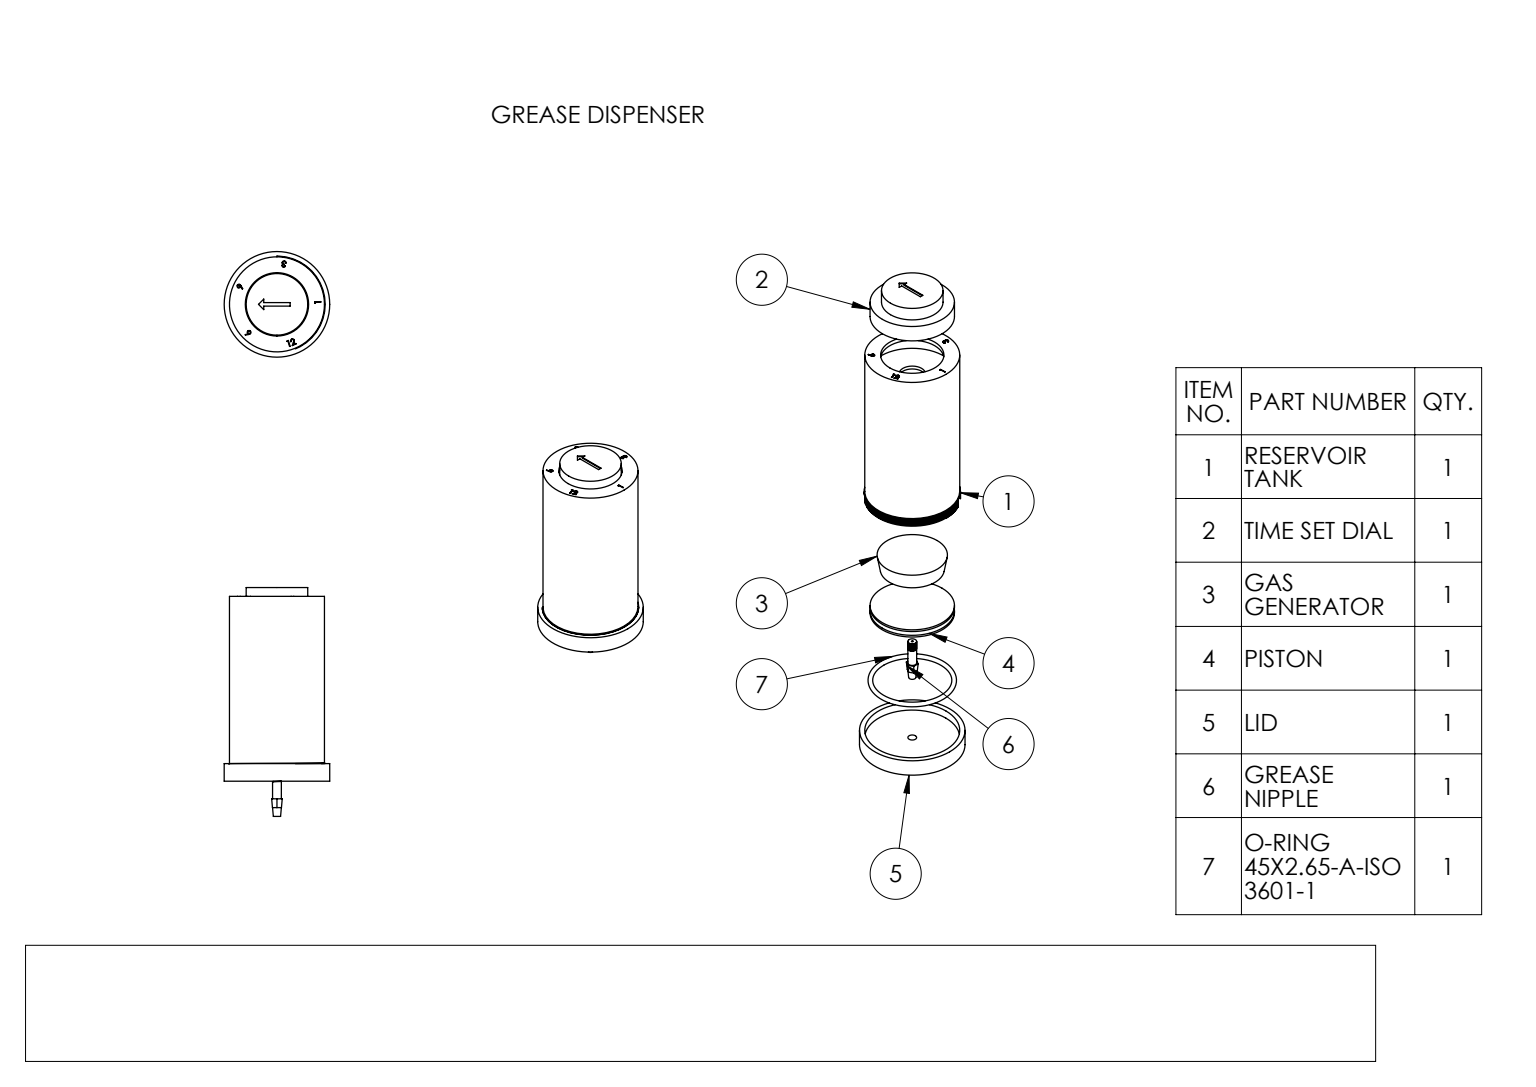
ISO-10303-21;
HEADER;
FILE_DESCRIPTION (('STEP AP214'),
    '1' );
FILE_NAME ('MAS-199',
    '2026-10-24T15:06:47',
    ( '' ),
    ( '' ),
    'SwSTEP 2.0',
    'SolidWorks 2026',
    '' );
FILE_SCHEMA (( 'AUTOMOTIVE_DESIGN' ));
ENDSEC;

DATA;
#1 = PRODUCT_DEFINITION_SHAPE ( 'NONE', 'NONE',  #7805 ) ;
#2 = CARTESIAN_POINT ( 'NONE',  ( 0.000000000000000000, 72.50000000000001421, 0.000000000000000000 ) ) ;
#3 = CARTESIAN_POINT ( 'NONE',  ( 4.786228327491940187E-16, -2.728124999385483473, 2.605501347177161087 ) ) ;
#4 = CARTESIAN_POINT ( 'NONE',  ( -22.08823018108446234, 99.50000000000000000, -9.406177930363766038 ) ) ;
#5 = ORIENTED_EDGE ( 'NONE', *, *, #2695, .F. ) ;
#6 = EDGE_LOOP ( 'NONE', ( #8139, #8496, #8983, #2392 ) ) ;
#7 = CARTESIAN_POINT ( 'NONE',  ( 2.256430356249999658, -2.578124999385483118, -1.302750673588581432 ) ) ;
#8 = CARTESIAN_POINT ( 'NONE',  ( 11.36312591709336850, 1.799999998907525267, 27.43301269999999903 ) ) ;
#9 = EDGE_CURVE ( 'NONE', #2280, #2682, #6327, .T. ) ;
#10 = FILL_AREA_STYLE_COLOUR ( '', #10270 ) ;
#11 = LINE ( 'NONE', #3942, #5600 ) ;
#12 = ADVANCED_FACE ( 'NONE', ( #17 ), #758, .T. ) ;
#13 = CARTESIAN_POINT ( 'NONE',  ( -27.00000000000001421, 4.450000000000000178, 11.18376618407356382 ) ) ;
#14 = DIRECTION ( 'NONE',  ( 0.3918949146621865109, 0.000000000000000000, 0.9200099868272720860 ) ) ;
#15 = CARTESIAN_POINT ( 'NONE',  ( -21.07742585509981126, 99.49999999999998579, -10.85999754779651383 ) ) ;
#16 = CARTESIAN_POINT ( 'NONE',  ( 1.128215178125001161, -4.153124999385482852, 1.954126010382870815 ) ) ;
#17 = FACE_OUTER_BOUND ( 'NONE', #3726, .T. ) ;
#18 = CARTESIAN_POINT ( 'NONE',  ( -11.36312591709335962, 2.899999998907525356, -27.43301270000000258 ) ) ;
#19 = CARTESIAN_POINT ( 'NONE',  ( 4.295198626299898237, 99.50000000000001421, -24.68029520312135361 ) ) ;
#20 = CARTESIAN_POINT ( 'NONE',  ( 1.249999999999999334, -1.050000000000000044, -2.165063509461096825 ) ) ;
#21 = CARTESIAN_POINT ( 'NONE',  ( 1.128215178124999607, -3.103124999385482585, -1.954126010382871259 ) ) ;
#22 = CYLINDRICAL_SURFACE ( 'NONE', #5038, 2.499999999999999556 ) ;
#23 = CARTESIAN_POINT ( 'NONE',  ( -22.51767453479306980, 100.0000000000000000, -9.764155749770198511 ) ) ;
#24 = FACE_OUTER_BOUND ( 'NONE', #4526, .T. ) ;
#25 = CARTESIAN_POINT ( 'NONE',  ( 1.250000000000001110, -2.043749998770965970, 2.165063509461096380 ) ) ;
#26 = VERTEX_POINT ( 'NONE', #3950 ) ;
#27 = CARTESIAN_POINT ( 'NONE',  ( 1.249999999999999334, -0.9937499987709658145, -2.165063509461096825 ) ) ;
#28 = CARTESIAN_POINT ( 'NONE',  ( -2.499999999999999112, -3.112499999999999822, 1.443375672974065882 ) ) ;
#29 = CARTESIAN_POINT ( 'NONE',  ( -14.97509118869195888, 99.99999999999998579, 15.26515554624281101 ) ) ;
#30 = CARTESIAN_POINT ( 'NONE',  ( 4.786228327491941173E-16, -3.178124999385482763, 2.605501347177161087 ) ) ;
#31 = ORIENTED_EDGE ( 'NONE', *, *, #3987, .F. ) ;
#32 = CIRCLE ( 'NONE', #8383, 30.00000000000000000 ) ;
#33 = AXIS2_PLACEMENT_3D ( 'NONE', #2920, #5329, #6943 ) ;
#34 = ORIENTED_EDGE ( 'NONE', *, *, #3622, .T. ) ;
#35 = CARTESIAN_POINT ( 'NONE',  ( -22.31230063665282515, 99.99999999999997158, -10.62159318200525249 ) ) ;
#36 = DIRECTION ( 'NONE',  ( 0.000000000000000000, 1.000000000000000000, 0.000000000000000000 ) ) ;
#37 = CARTESIAN_POINT ( 'NONE',  ( 1.034219503716432668E-14, -3.656249998770965792, -2.500000000000000000 ) ) ;
#38 = CARTESIAN_POINT ( 'NONE',  ( 27.00000000000000355, 2.999999997815050889, 0.000000000000000000 ) ) ;
#39 = CARTESIAN_POINT ( 'NONE',  ( 19.39806930854667399, 3.449999998907525622, 19.39806930854668465 ) ) ;
#40 = AXIS2_PLACEMENT_3D ( 'NONE', #3682, #8497, #6028 ) ;
#41 = EDGE_LOOP ( 'NONE', ( #10357, #6514, #2134, #4776 ) ) ;
#42 = EDGE_CURVE ( 'NONE', #3838, #8637, #9238, .T. ) ;
#43 = CARTESIAN_POINT ( 'NONE',  ( 3.739209042966563867, 99.50000000000000000, -21.42288334414699236 ) ) ;
#44 = ITEM_DEFINED_TRANSFORMATION ( 'NONE', 'NONE', #5307,  #5055 ) ;
#45 = CARTESIAN_POINT ( 'NONE',  ( 3.873456569393397331, 100.0000000000000284, -22.53291374702356364 ) ) ;
#46 = CARTESIAN_POINT ( 'NONE',  ( -2.256430356249999214, -3.365624999385482319, 1.302750673588581876 ) ) ;
#47 = CARTESIAN_POINT ( 'NONE',  ( -21.28703419482447146, 99.49999999999997158, -11.01737971290317297 ) ) ;
#48 = CARTESIAN_POINT ( 'NONE',  ( 11.36312591709336139, 5.299999998907526155, -27.43301270000000258 ) ) ;
#49 = UNCERTAINTY_MEASURE_WITH_UNIT (LENGTH_MEASURE( 1.000000000000000082E-05 ), #5358, 'distance_accuracy_value', 'NONE');
#50 = AXIS2_PLACEMENT_3D ( 'NONE', #9695, #1591, #1737 ) ;
#51 = CARTESIAN_POINT ( 'NONE',  ( -15.10382517959271098, 99.49999999999998579, 15.91526905993627317 ) ) ;
#52 = DIRECTION ( 'NONE',  ( 0.4750403377899758972, 0.000000000000000000, -0.8799640205556052974 ) ) ;
#53 = CARTESIAN_POINT ( 'NONE',  ( 0.000000000000000000, 85.00000000000000000, -20.00000000000000000 ) ) ;
#54 = CARTESIAN_POINT ( 'NONE',  ( 3.061616997868383141E-16, 0.000000000000000000, 2.500000000000000000 ) ) ;
#55 = CARTESIAN_POINT ( 'NONE',  ( -1.128215178124998497, -3.665624999385482585, 1.954126010382872147 ) ) ;
#56 = CARTESIAN_POINT ( 'NONE',  ( 9.910564025336874749, 100.0000000000000142, 20.75459158945058036 ) ) ;
#57 = ORIENTED_EDGE ( 'NONE', *, *, #3072, .T. ) ;
#58 = ADVANCED_FACE ( 'NONE', ( #3173 ), #2520, .T. ) ;
#59 = ORIENTED_EDGE ( 'NONE', *, *, #4217, .F. ) ;
#60 = CARTESIAN_POINT ( 'NONE',  ( -2.256430356250000102, -1.940624999385482941, 0.000000000000000000 ) ) ;
#61 = CARTESIAN_POINT ( 'NONE',  ( 27.43301270000000258, 1.999999998907524779, -11.36312591709336139 ) ) ;
#62 = FILL_AREA_STYLE ('',( #10 ) ) ;
#63 = CARTESIAN_POINT ( 'NONE',  ( 1.679787559701184688E-15, 5.249999998907525445, -27.43301270000000258 ) ) ;
#64 = AXIS2_PLACEMENT_3D ( 'NONE', #1231, #6667, #8456 ) ;
#65 = CARTESIAN_POINT ( 'NONE',  ( 11.18376618407356915, 4.950000000000000178, -27.00000000000000355 ) ) ;
#66 = FACE_OUTER_BOUND ( 'NONE', #7305, .T. ) ;
#67 = CARTESIAN_POINT ( 'NONE',  ( -16.33590634957226229, 99.50000000000000000, 16.80570853669505382 ) ) ;
#68 = CARTESIAN_POINT ( 'NONE',  ( -20.91264567078791714, 99.99999999999994316, -10.54226115003387676 ) ) ;
#69 = EDGE_CURVE ( 'NONE', #5685, #7937, #6333, .T. ) ;
#70 = ORIENTED_EDGE ( 'NONE', *, *, #9652, .T. ) ;
#71 = ORIENTED_EDGE ( 'NONE', *, *, #3469, .T. ) ;
#72 = CARTESIAN_POINT ( 'NONE',  ( 3.551917533706515417, 100.0000000000000142, -21.11785906961830150 ) ) ;
#73 = ORIENTED_EDGE ( 'NONE', *, *, #5083, .F. ) ;
#74 = ADVANCED_FACE ( 'NONE', ( #2725 ), #8325, .T. ) ;
#75 = CARTESIAN_POINT ( 'NONE',  ( 27.43301269999999548, 4.199999998907525622, 11.36312591709337916 ) ) ;
#76 = FACE_OUTER_BOUND ( 'NONE', #1497, .T. ) ;
#77 = CARTESIAN_POINT ( 'NONE',  ( 9.877377282685029372E-16, -1.237499999999999600, 2.500000000000000000 ) ) ;
#78 = CARTESIAN_POINT ( 'NONE',  ( 2.256430356250000546, -4.565624999385482496, 1.302750673588579877 ) ) ;
#79 = CARTESIAN_POINT ( 'NONE',  ( -4.357666448243394824E-15, -2.531249998770965348, 2.500000000000000000 ) ) ;
#80 = EDGE_CURVE ( 'NONE', #2765, #6040, #6971, .T. ) ;
#81 = CARTESIAN_POINT ( 'NONE',  ( -22.63784607493503387, 99.50000000000001421, -10.71517552924587058 ) ) ;
#82 = AXIS2_PLACEMENT_3D ( 'NONE', #9543, #4773, #8119 ) ;
#83 = CARTESIAN_POINT ( 'NONE',  ( -1.250000000000000222, -4.518749998770965171, -2.165063509461096825 ) ) ;
#84 = VERTEX_POINT ( 'NONE', #3619 ) ;
#85 = EDGE_CURVE ( 'NONE', #5894, #5272, #1155, .T. ) ;
#86 = CARTESIAN_POINT ( 'NONE',  ( 1.653273178848927064E-15, 2.399999997815050357, -27.00000000000000355 ) ) ;
#87 = CARTESIAN_POINT ( 'NONE',  ( -20.71654887124055122, 99.50000000000001421, -9.874326132881018125 ) ) ;
#88 = LINE ( 'NONE', #2497, #4362 ) ;
#89 = CARTESIAN_POINT ( 'NONE',  ( 2.256430356249999658, -3.928124999385482319, -1.302750673588581432 ) ) ;
#90 = B_SPLINE_SURFACE_WITH_KNOTS ( 'NONE', 3, 1, ( 
 ( #3080, #5199 ),
 ( #8397, #1229 ),
 ( #4422, #5539 ),
 ( #1701, #10302 ),
 ( #3282, #3232 ),
 ( #4117, #7200 ),
 ( #3911, #924 ),
 ( #4848, #7097 ),
 ( #4064, #3134 ),
 ( #2291, #2443 ),
 ( #6321, #139 ) ),
 .UNSPECIFIED., .F., .F., .F.,
 ( 4, 1, 1, 1, 1, 1, 1, 1, 4 ),
 ( 2, 2 ),
 ( 0.000000000000000000, 0.09809051273808343241, 0.1997563395654988194, 0.3058527769869914259, 0.4162847437678430240, 0.5377099880548563693, 0.6743560419832976827, 0.8289895874771281425, 1.000000000000000000 ),
 ( 0.000000000000000000, 1.000000000000000000 ),
 .UNSPECIFIED. ) ;
#91 = CARTESIAN_POINT ( 'NONE',  ( 3.058419780146050648, 99.50000000000000000, -23.12871267107006545 ) ) ;
#92 = ORIENTED_EDGE ( 'NONE', *, *, #2350, .T. ) ;
#93 = AXIS2_PLACEMENT_3D ( 'NONE', #4532, #670, #7729 ) ;
#94 = CARTESIAN_POINT ( 'NONE',  ( -15.22320097062094568, 99.50000000000001421, 16.32303119091969634 ) ) ;
#95 = CARTESIAN_POINT ( 'NONE',  ( -2.499999999999999112, -3.506249998770964993, 1.443375672974065882 ) ) ;
#96 = CARTESIAN_POINT ( 'NONE',  ( 0.000000000000000000, 100.0000000000000000, 0.000000000000000000 ) ) ;
#97 = CARTESIAN_POINT ( 'NONE',  ( 9.245739950628269810, 100.0000000000000284, 20.03726560014620617 ) ) ;
#98 = ORIENTED_EDGE ( 'NONE', *, *, #7857, .T. ) ;
#99 = CARTESIAN_POINT ( 'NONE',  ( 0.000000000000000000, 0.000000000000000000, 0.000000000000000000 ) ) ;
#100 = VECTOR ( 'NONE', #6339, 1000.000000000000000 ) ;
#101 = CARTESIAN_POINT ( 'NONE',  ( -20.89169796687544789, 100.0000000000000142, -10.40078880447404330 ) ) ;
#102 = CARTESIAN_POINT ( 'NONE',  ( -2.256430356250000102, -0.1781249993854829572, -1.302750673588580321 ) ) ;
#103 = EDGE_CURVE ( 'NONE', #3372, #2494, #7434, .T. ) ;
#104 = FACE_OUTER_BOUND ( 'NONE', #9219, .T. ) ;
#105 = CARTESIAN_POINT ( 'NONE',  ( 27.43301269999999548, 5.099999998907525978, 11.36312591709337738 ) ) ;
#106 = CARTESIAN_POINT ( 'NONE',  ( -15.19031985176477662, 99.49999999999998579, 15.56880617076518547 ) ) ;
#107 = DIRECTION ( 'NONE',  ( 0.000000000000000000, 0.000000000000000000, 1.000000000000000000 ) ) ;
#108 = CARTESIAN_POINT ( 'NONE',  ( -15.37123125604856710, 99.50000000000001421, 16.48683530611566539 ) ) ;
#109 = DIRECTION ( 'NONE',  ( 4.336808689942017736E-16, 0.000000000000000000, -1.000000000000000000 ) ) ;
#110 = CARTESIAN_POINT ( 'NONE',  ( -1.128215178124998497, -4.115624999385482319, 1.954126010382872147 ) ) ;
#111 = CARTESIAN_POINT ( 'NONE',  ( 3.970307086022987431, 99.50000000000001421, -24.36314111580913178 ) ) ;
#112 = EDGE_LOOP ( 'NONE', ( #9331, #6596, #10060, #487 ) ) ;
#113 = ORIENTED_EDGE ( 'NONE', *, *, #6148, .T. ) ;
#114 = CARTESIAN_POINT ( 'NONE',  ( -1.128215178124998497, -3.665624999385482585, 1.954126010382872147 ) ) ;
#115 = CARTESIAN_POINT ( 'NONE',  ( 27.43301270000000258, 1.149999998907525356, 0.000000000000000000 ) ) ;
#116 = CARTESIAN_POINT ( 'NONE',  ( 0.000000000000000000, 0.000000000000000000, 0.000000000000000000 ) ) ;
#117 = FACE_OUTER_BOUND ( 'NONE', #7334, .T. ) ;
#118 = CARTESIAN_POINT ( 'NONE',  ( -27.43301270000000258, 0.6499999989075253559, -3.359575119402369376E-15 ) ) ;
#119 = DIRECTION ( 'NONE',  ( -0.000000000000000000, -1.000000000000000000, -0.000000000000000000 ) ) ;
#120 = ORIENTED_EDGE ( 'NONE', *, *, #3091, .T. ) ;
#121 = EDGE_CURVE ( 'NONE', #3756, #7561, #4966, .T. ) ;
#122 = VECTOR ( 'NONE', #1890, 999.9999999999998863 ) ;
#123 = CARTESIAN_POINT ( 'NONE',  ( 0.000000000000000000, 99.50000000000000000, 0.000000000000000000 ) ) ;
#124 = FACE_OUTER_BOUND ( 'NONE', #10204, .T. ) ;
#125 = ORIENTED_EDGE ( 'NONE', *, *, #7390, .T. ) ;
#126 = ORIENTED_EDGE ( 'NONE', *, *, #1417, .F. ) ;
#127 = CARTESIAN_POINT ( 'NONE',  ( 1.250000000000001110, -5.193749998770964993, 2.165063509461096380 ) ) ;
#128 = CARTESIAN_POINT ( 'NONE',  ( 19.39806930854667399, 4.949999998907525622, 19.39806930854668465 ) ) ;
#129 = CARTESIAN_POINT ( 'NONE',  ( 3.538198506519217190, 99.99999999999998579, -24.58220198924426114 ) ) ;
#130 = CARTESIAN_POINT ( 'NONE',  ( -2.256430356250000102, -4.303124999385482319, 0.000000000000000000 ) ) ;
#131 = CARTESIAN_POINT ( 'NONE',  ( -16.49419651247312046, 99.99999999999998579, 15.57134447358898477 ) ) ;
#132 = CARTESIAN_POINT ( 'NONE',  ( -22.69253165798458127, 100.0000000000000142, -10.28928739654909563 ) ) ;
#133 = CARTESIAN_POINT ( 'NONE',  ( 4.331079892889020400, 100.0000000000000000, -24.67336562508343079 ) ) ;
#134 = AXIS2_PLACEMENT_3D ( 'NONE', #8588, #6169, #2769 ) ;
#135 = CARTESIAN_POINT ( 'NONE',  ( -1.249999999999998224, -4.368749998770964815, 2.165063509461097713 ) ) ;
#136 = ORIENTED_EDGE ( 'NONE', *, *, #3638, .F. ) ;
#137 = ORIENTED_EDGE ( 'NONE', *, *, #6348, .F. ) ;
#138 = FACE_OUTER_BOUND ( 'NONE', #6423, .T. ) ;
#139 = CARTESIAN_POINT ( 'NONE',  ( -16.07368679829020763, 100.0000000000000000, 17.11560437002838952 ) ) ;
#140 = CARTESIAN_POINT ( 'NONE',  ( -14.74935495356232984, 100.0000000000000142, 15.91322402822111926 ) ) ;
#141 = CARTESIAN_POINT ( 'NONE',  ( -1.128215178125000273, -3.815624999385482941, -1.954126010382871259 ) ) ;
#142 = ADVANCED_FACE ( 'NONE', ( #1039 ), #6680, .T. ) ;
#143 = EDGE_CURVE ( 'NONE', #8324, #1908, #2115, .T. ) ;
#144 = AXIS2_PLACEMENT_3D ( 'NONE', #2203, #6849, #5404 ) ;
#145 = LINE ( 'NONE', #6521, #2502 ) ;
#146 = DIRECTION ( 'NONE',  ( -1.000000000000000000, -0.000000000000000000, -0.000000000000000000 ) ) ;
#147 = CARTESIAN_POINT ( 'NONE',  ( 1.250000000000001110, -3.843749998770965348, 2.165063509461096380 ) ) ;
#148 = CARTESIAN_POINT ( 'NONE',  ( -19.09188309203678813, 4.500000000000000888, 19.09188309203678457 ) ) ;
#149 = EDGE_LOOP ( 'NONE', ( #7106, #3257, #2787, #8826 ) ) ;
#150 = CARTESIAN_POINT ( 'NONE',  ( 3.411785164761435674, 99.50000000000000000, -22.76693382491622231 ) ) ;
#151 = CARTESIAN_POINT ( 'NONE',  ( 3.750007936853901658, 99.99999999999998579, -22.95001988029826734 ) ) ;
#152 = CARTESIAN_POINT ( 'NONE',  ( 7.856939908706818798, 99.50000000000001421, 20.19612520319305560 ) ) ;
#153 = DIRECTION ( 'NONE',  ( -0.000000000000000000, -0.000000000000000000, -1.000000000000000000 ) ) ;
#154 = CARTESIAN_POINT ( 'NONE',  ( 27.43301270000000258, 4.349999998907525089, 0.000000000000000000 ) ) ;
#155 = CARTESIAN_POINT ( 'NONE',  ( 26.99999999999999645, 3.150000000000000799, 11.18376618407358691 ) ) ;
#156 = CARTESIAN_POINT ( 'NONE',  ( -21.24882413972086681, 100.0000000000000284, -9.742484589929601313 ) ) ;
#157 = CARTESIAN_POINT ( 'NONE',  ( 3.717146347979291665, 99.50000000000000000, -21.42716062222556417 ) ) ;
#158 = CARTESIAN_POINT ( 'NONE',  ( 3.681717055787076642, 99.50000000000000000, -21.09125273517263111 ) ) ;
#159 = CARTESIAN_POINT ( 'NONE',  ( 1.034219503716432668E-14, -4.612500000000000711, -2.500000000000000000 ) ) ;
#160 = ORIENTED_EDGE ( 'NONE', *, *, #2379, .T. ) ;
#161 = CARTESIAN_POINT ( 'NONE',  ( -2.256430356249999214, -4.153124999385482852, 1.302750673588581876 ) ) ;
#162 = CARTESIAN_POINT ( 'NONE',  ( -16.01161620991261358, 99.50000000000000000, 17.10240122391520146 ) ) ;
#163 = B_SPLINE_CURVE_WITH_KNOTS ( 'NONE', 3,
 ( #932, #5497, #832, #3193, #8885, #3093, #3922, #8786, #6277, #3240, #8737, #729, #9473, #2452, #4752 ),
 .UNSPECIFIED., .F., .F.,
 ( 4, 1, 1, 1, 1, 1, 1, 1, 1, 1, 1, 1, 4 ),
 ( 0.000000000000000000, 0.08490232564366416435, 0.1680779112633816463, 0.2506304657828534177, 0.3338427399641299420, 0.4169763759729993580, 0.4990117930239920674, 0.5811067191809071719, 0.6656374296971073745, 0.7500328835558887075, 0.8331455368193440014, 0.9159638734519762737, 1.000000000000000000 ),
 .UNSPECIFIED. ) ;
#164 = CARTESIAN_POINT ( 'NONE',  ( 11.18376618407357626, 3.049999999999999822, 27.00000000000000000 ) ) ;
#165 = CARTESIAN_POINT ( 'NONE',  ( 3.373335371007685435, 99.50000000000000000, -22.75111425220066863 ) ) ;
#166 = CARTESIAN_POINT ( 'NONE',  ( 6.307557144418638510E-17, -20.00000000000000000, -2.958985580760425727 ) ) ;
#167 = CARTESIAN_POINT ( 'NONE',  ( 1.250000000000001110, -3.449999999999999289, 2.165063509461096380 ) ) ;
#168 = CARTESIAN_POINT ( 'NONE',  ( -21.07742585509981126, 99.99999999999995737, -10.85999754779651383 ) ) ;
#169 = ORIENTED_EDGE ( 'NONE', *, *, #6403, .F. ) ;
#170 = CARTESIAN_POINT ( 'NONE',  ( 1.249999999999999334, -1.443749998770965881, -2.165063509461096825 ) ) ;
#171 = CARTESIAN_POINT ( 'NONE',  ( 2.500000000000000000, -4.218749998770966236, -3.061616997868383141E-16 ) ) ;
#172 = EDGE_CURVE ( 'NONE', #957, #2983, #5656, .T. ) ;
#173 = CARTESIAN_POINT ( 'NONE',  ( -1.128215178125000273, -4.828124999385481786, -1.954126010382871259 ) ) ;
#174 = CARTESIAN_POINT ( 'NONE',  ( 9.404665101723468368, 99.50000000000000000, 20.17141824467128686 ) ) ;
#175 = CARTESIAN_POINT ( 'NONE',  ( -16.87593989452418697, 99.49999999999998579, 15.58794934546231126 ) ) ;
#176 = CARTESIAN_POINT ( 'NONE',  ( 8.064245308217579122, 99.99999999999998579, 20.64099956338070641 ) ) ;
#177 = SHAPE_REPRESENTATION ( 'piston', ( #5055 ), #738 ) ;
#178 = CARTESIAN_POINT ( 'NONE',  ( -1.250000000000000222, -3.618749998770965259, -2.165063509461096825 ) ) ;
#179 = ORIENTED_EDGE ( 'NONE', *, *, #6506, .T. ) ;
#180 = ORIENTED_EDGE ( 'NONE', *, *, #3035, .T. ) ;
#181 = EDGE_CURVE ( 'NONE', #471, #3838, #8521, .T. ) ;
#182 = CARTESIAN_POINT ( 'NONE',  ( -22.29247428061501779, 99.99999999999997158, -10.66603791136541624 ) ) ;
#183 = CARTESIAN_POINT ( 'NONE',  ( 3.611424427577684781, 99.99999999999998579, -21.45475674085064099 ) ) ;
#184 = EDGE_CURVE ( 'NONE', #533, #5989, #307, .T. ) ;
#185 = CARTESIAN_POINT ( 'NONE',  ( -15.07178375341841381, 100.0000000000000000, 16.66969090848992607 ) ) ;
#186 = CARTESIAN_POINT ( 'NONE',  ( 1.128215178125001161, -4.490624999385482319, 1.954126010382870815 ) ) ;
#187 = ORIENTED_EDGE ( 'NONE', *, *, #7681, .T. ) ;
#188 = DIRECTION ( 'NONE',  ( 0.000000000000000000, -1.000000000000000000, 0.000000000000000000 ) ) ;
#189 = PRODUCT_RELATED_PRODUCT_CATEGORY ( 'part', '', ( #8779 ) ) ;
#190 = DIRECTION ( 'NONE',  ( -0.05422338932609765960, 0.000000000000000000, -0.9985288298541962204 ) ) ;
#191 = EDGE_CURVE ( 'NONE', #3656, #1900, #9595, .T. ) ;
#192 = PLANE ( 'NONE',  #10324 ) ;
#193 = ORIENTED_EDGE ( 'NONE', *, *, #8350, .T. ) ;
#194 = ADVANCED_FACE ( 'NONE', ( #1864 ), #9727, .F. ) ;
#195 = CARTESIAN_POINT ( 'NONE',  ( 3.302864939465488536, 99.50000000000001421, -22.83905924565489443 ) ) ;
#196 = CARTESIAN_POINT ( 'NONE',  ( 3.891852272358404807, 99.99999999999998579, -22.89765557720719968 ) ) ;
#197 = CARTESIAN_POINT ( 'NONE',  ( 6.123233995736709336E-17, -25.00000000000000000, 0.4999999999999953371 ) ) ;
#198 = EDGE_LOOP ( 'NONE', ( #2371, #2144, #704, #4706 ) ) ;
#199 = CARTESIAN_POINT ( 'NONE',  ( 3.207057600658871355, 100.0000000000000284, -22.07913334414698880 ) ) ;
#200 = CARTESIAN_POINT ( 'NONE',  ( 27.00000000000000355, 2.999999997815050889, 0.000000000000000000 ) ) ;
#201 = CARTESIAN_POINT ( 'NONE',  ( -20.71654887124055122, 100.0000000000000142, -9.874326132881018125 ) ) ;
#202 = CARTESIAN_POINT ( 'NONE',  ( -21.66466628782423243, 100.0000000000000142, -9.640935998098070669 ) ) ;
#203 = LINE ( 'NONE', #3388, #8398 ) ;
#204 = VECTOR ( 'NONE', #9185, 1000.000000000000000 ) ;
#205 = LINE ( 'NONE', #1725, #6091 ) ;
#206 = CARTESIAN_POINT ( 'NONE',  ( -0.6698729810778081273, -2.157596189432334111, 2.499999999999999112 ) ) ;
#207 = ORIENTED_EDGE ( 'NONE', *, *, #9006, .F. ) ;
#208 = CARTESIAN_POINT ( 'NONE',  ( 2.256430356250000546, -4.003124999385482496, 1.302750673588579877 ) ) ;
#209 = FACE_OUTER_BOUND ( 'NONE', #3870, .T. ) ;
#210 = CARTESIAN_POINT ( 'NONE',  ( 9.806436918512124734, 99.99999999999998579, 20.18080982695387604 ) ) ;
#211 = VECTOR ( 'NONE', #9822, 1000.000000000000000 ) ;
#212 = CARTESIAN_POINT ( 'NONE',  ( -27.43301270000000258, 2.199999998907525622, -11.36312591709336317 ) ) ;
#213 = CARTESIAN_POINT ( 'NONE',  ( 2.500000000000000000, -0.6187499987709659255, -3.061616997868383141E-16 ) ) ;
#214 = DIRECTION ( 'NONE',  ( -0.000000000000000000, 1.000000000000000000, -0.000000000000000000 ) ) ;
#215 = CARTESIAN_POINT ( 'NONE',  ( 8.429066232339796017, 100.0000000000000000, 19.67794530653910101 ) ) ;
#216 = CARTESIAN_POINT ( 'NONE',  ( 1.653273178848927064E-15, 2.399999997815050357, -27.00000000000000355 ) ) ;
#217 = ORIENTED_EDGE ( 'NONE', *, *, #7917, .F. ) ;
#218 = CARTESIAN_POINT ( 'NONE',  ( -20.89052720883767122, 99.50000000000000000, -9.602653601535816819 ) ) ;
#219 = CARTESIAN_POINT ( 'NONE',  ( 11.36312591709336139, 5.199999998907525622, -27.43301270000000258 ) ) ;
#220 = CARTESIAN_POINT ( 'NONE',  ( -16.18965924272485779, 99.49999999999998579, 15.26525457555968224 ) ) ;
#221 = FACE_OUTER_BOUND ( 'NONE', #8631, .T. ) ;
#222 = CARTESIAN_POINT ( 'NONE',  ( 2.500000000000000444, -2.456249998770965615, 1.443375672974063439 ) ) ;
#223 = CARTESIAN_POINT ( 'NONE',  ( 26.99999999999999645, 1.550000000000000266, 11.18376618407358691 ) ) ;
#224 = VERTEX_POINT ( 'NONE', #1816 ) ;
#225 = CARTESIAN_POINT ( 'NONE',  ( 5.240996349771887886, 100.0000000000000142, -23.60769396873743631 ) ) ;
#226 = ORIENTED_EDGE ( 'NONE', *, *, #3625, .T. ) ;
#227 = EDGE_CURVE ( 'NONE', #6767, #4694, #1090, .T. ) ;
#228 = CARTESIAN_POINT ( 'NONE',  ( 1.249999999999999334, -5.043749998770965526, -2.165063509461096825 ) ) ;
#229 = VERTEX_POINT ( 'NONE', #4281 ) ;
#230 = ORIENTED_EDGE ( 'NONE', *, *, #6289, .F. ) ;
#231 = LINE ( 'NONE', #3414, #2289 ) ;
#232 = LINE ( 'NONE', #8144, #5785 ) ;
#233 = CARTESIAN_POINT ( 'NONE',  ( -22.11394672483139701, 99.50000000000000000, -10.91855052283267646 ) ) ;
#234 =( BOUNDED_CURVE ( )  B_SPLINE_CURVE ( 1, ( #10186, #707 ),
 .UNSPECIFIED., .F., .F. ) 
 B_SPLINE_CURVE_WITH_KNOTS ( ( 2, 2 ),
 ( 0.000000000000000000, 1.000000000000000000 ),
 .UNSPECIFIED. ) 
 CURVE ( )  GEOMETRIC_REPRESENTATION_ITEM ( )  RATIONAL_B_SPLINE_CURVE ( ( 0.9401538480137057174, 0.9401538480137057174 ) ) 
 REPRESENTATION_ITEM ( '' )  );
#235 = CARTESIAN_POINT ( 'NONE',  ( -15.26676860252058887, 99.99999999999998579, 16.38168943497750973 ) ) ;
#236 = VECTOR ( 'NONE', #2101, 1000.000000000000000 ) ;
#237 = EDGE_CURVE ( 'NONE', #1790, #7639, #6949, .T. ) ;
#238 = DIRECTION ( 'NONE',  ( 0.000000000000000000, 0.000000000000000000, -1.000000000000000000 ) ) ;
#239 = DIRECTION ( 'NONE',  ( 0.000000000000000000, -1.000000000000000000, 0.000000000000000000 ) ) ;
#240 = CARTESIAN_POINT ( 'NONE',  ( 0.000000000000000000, 97.50000000000000000, 18.00000000000000000 ) ) ;
#241 = ORIENTED_EDGE ( 'NONE', *, *, #4209, .F. ) ;
#242 = CARTESIAN_POINT ( 'NONE',  ( 3.058419780146050648, 99.50000000000000000, -23.12871267107006545 ) ) ;
#243 = LINE ( 'NONE', #5946, #5211 ) ;
#244 = CARTESIAN_POINT ( 'NONE',  ( 3.701176614148623756, 99.50000000000000000, -24.64875008328975170 ) ) ;
#245 = CARTESIAN_POINT ( 'NONE',  ( 7.734522023158566739, 99.50000000000002842, 20.86022014488863618 ) ) ;
#246 = ORIENTED_EDGE ( 'NONE', *, *, #1140, .T. ) ;
#247 = CARTESIAN_POINT ( 'NONE',  ( 0.000000000000000000, 73.81339255365637086, 0.000000000000000000 ) ) ;
#248 = CARTESIAN_POINT ( 'NONE',  ( 1.653273178848927064E-15, 4.799999997815051600, -27.00000000000000355 ) ) ;
#249 = CARTESIAN_POINT ( 'NONE',  ( -21.00001322343447541, 99.50000000000001421, -9.990026185521596602 ) ) ;
#250 = CARTESIAN_POINT ( 'NONE',  ( 3.635130212803377781, 100.0000000000000000, -23.00575896550913768 ) ) ;
#251 = CARTESIAN_POINT ( 'NONE',  ( -21.72555844818415594, 99.50000000000001421, -11.09629251537910655 ) ) ;
#252 = CARTESIAN_POINT ( 'NONE',  ( 4.906732565843439531, 100.0000000000000142, -23.57187248890526376 ) ) ;
#253 = CARTESIAN_POINT ( 'NONE',  ( -1.250000000000000222, -2.324999999999999734, -2.165063509461096825 ) ) ;
#254 = VECTOR ( 'NONE', #2667, 1000.000000000000000 ) ;
#255 = B_SPLINE_CURVE_WITH_KNOTS ( 'NONE', 3,
 ( #43, #4128, #5748, #6482, #981, #3244, #8984, #8105, #7258, #4950, #7354, #5651, #9812, #9671, #7311 ),
 .UNSPECIFIED., .F., .F.,
 ( 4, 1, 1, 1, 1, 1, 1, 1, 1, 1, 1, 1, 4 ),
 ( 0.000000000000000000, 0.1166921615859537187, 0.2277195327244859735, 0.3361971884410420164, 0.4453256767247914527, 0.5018483577356800396, 0.5617326728321133666, 0.6243107931132723110, 0.6909729641497043273, 0.7615676753376537933, 0.8363829297815326136, 0.9156607463298391814, 0.9999999999999998890 ),
 .UNSPECIFIED. ) ;
#256 = CARTESIAN_POINT ( 'NONE',  ( -2.256430356250000546, -5.114265350234221685, -0.8212662131217605133 ) ) ;
#257 = SURFACE_STYLE_USAGE ( .BOTH. , #8210 ) ;
#258 = CARTESIAN_POINT ( 'NONE',  ( -15.03963071504896121, 100.0000000000000000, 16.63526396357264758 ) ) ;
#259 = CIRCLE ( 'NONE', #7786, 2.500000000000000000 ) ;
#260 = CARTESIAN_POINT ( 'NONE',  ( 0.000000000000000000, 5.000000000000000000, -30.00000000000000000 ) ) ;
#261 = CARTESIAN_POINT ( 'NONE',  ( 27.43301270000000258, 1.849999998907525534, 0.000000000000000000 ) ) ;
#262 = LINE ( 'NONE', #2027, #6876 ) ;
#263 = ADVANCED_FACE ( 'NONE', ( #4540 ), #1407, .T. ) ;
#264 = CARTESIAN_POINT ( 'NONE',  ( -20.64578974631102426, 99.99999999999995737, -10.10077944494247504 ) ) ;
#265 = DIRECTION ( 'NONE',  ( -0.000000000000000000, 1.000000000000000000, -0.000000000000000000 ) ) ;
#266 = CARTESIAN_POINT ( 'NONE',  ( 8.322475189980043098, 100.0000000000000142, 19.72675386960232657 ) ) ;
#267 = ORIENTED_EDGE ( 'NONE', *, *, #2370, .F. ) ;
#268 = CARTESIAN_POINT ( 'NONE',  ( -21.30033281797529909, 99.50000000000002842, -9.345151174687854834 ) ) ;
#269 = CARTESIAN_POINT ( 'NONE',  ( 4.135809822336132591, 99.99999999999998579, -24.70305975188825443 ) ) ;
#270 = DIRECTION ( 'NONE',  ( 0.000000000000000000, -1.000000000000000000, 0.000000000000000000 ) ) ;
#271 = CARTESIAN_POINT ( 'NONE',  ( 3.775125937424839151, 100.0000000000000000, -21.41825520325024712 ) ) ;
#272 = CARTESIAN_POINT ( 'NONE',  ( 8.829292973371666520, 99.49999999999998579, 19.92220432019063736 ) ) ;
#273 = CARTESIAN_POINT ( 'NONE',  ( 0.000000000000000000, 0.000000000000000000, -2.500000000000000000 ) ) ;
#274 = CIRCLE ( 'NONE', #2111, 2.499999999999999556 ) ;
#275 = CARTESIAN_POINT ( 'NONE',  ( 0.000000000000000000, 75.00000000000001421, 0.000000000000000000 ) ) ;
#276 = CARTESIAN_POINT ( 'NONE',  ( 4.786228327491941173E-16, -0.5906249993854828517, 2.605501347177161087 ) ) ;
#277 = ORIENTED_EDGE ( 'NONE', *, *, #5688, .F. ) ;
#278 = ORIENTED_EDGE ( 'NONE', *, *, #3961, .T. ) ;
#279 = VECTOR ( 'NONE', #5092, 1000.000000000000000 ) ;
#280 = CYLINDRICAL_SURFACE ( 'NONE', #8136, 0.4999999999999953371 ) ;
#281 = CARTESIAN_POINT ( 'NONE',  ( 6.246869686064662197, 99.50000000000000000, 20.92172973853146090 ) ) ;
#282 = CARTESIAN_POINT ( 'NONE',  ( 1.653273178848927064E-15, 4.799999997815051600, -27.00000000000000355 ) ) ;
#283 = DIRECTION ( 'NONE',  ( 8.881784197001252323E-16, 0.000000000000000000, 1.000000000000000000 ) ) ;
#284 = COLOUR_RGB ( '',1.000000000000000000, 0.9490196078431372140, 0.9098039215686274384 ) ;
#285 = CARTESIAN_POINT ( 'NONE',  ( 8.081885929396888102, 99.50000000000001421, 20.89785832093561169 ) ) ;
#286 = CARTESIAN_POINT ( 'NONE',  ( 2.852289972453743161, 99.50000000000000000, -22.14293542748032451 ) ) ;
#287 = CARTESIAN_POINT ( 'NONE',  ( 3.061616997868383141E-16, 0.000000000000000000, 2.500000000000000000 ) ) ;
#288 = CARTESIAN_POINT ( 'NONE',  ( 3.735769352376668184, 99.49999999999998579, -24.30643046864489420 ) ) ;
#289 =( BOUNDED_CURVE ( )  B_SPLINE_CURVE ( 2, ( #364, #2666, #6794, #9834, #213, #3555, #2617, #5222, #2774 ),
 .UNSPECIFIED., .F., .F. ) 
 B_SPLINE_CURVE_WITH_KNOTS ( ( 3, 2, 2, 2, 3 ),
 ( 0.02083333333333333218, 0.02777777777777777624, 0.04166666666666666435, 0.05555555555555555247, 0.06250000000000000000 ),
 .UNSPECIFIED. ) 
 CURVE ( )  GEOMETRIC_REPRESENTATION_ITEM ( )  RATIONAL_B_SPLINE_CURVE ( ( 0.9330127018922194093, 0.9330127018922194093, 1.000000000000000000, 0.8660254037844387076, 1.000000000000000000, 0.8660254037844387076, 1.000000000000000000, 0.9330127018922194093, 0.9330127018922194093 ) ) 
 REPRESENTATION_ITEM ( '' )  );
#290 = ORIENTED_EDGE ( 'NONE', *, *, #2409, .F. ) ;
#291 = DIRECTION ( 'NONE',  ( -0.000000000000000000, 1.000000000000000000, -0.000000000000000000 ) ) ;
#292 = CARTESIAN_POINT ( 'NONE',  ( -27.43301270000000258, 3.949999998907525178, -3.359575119402369376E-15 ) ) ;
#293 = CARTESIAN_POINT ( 'NONE',  ( -0.6698729810778054627, -2.101346188203299548, 2.500000000000000000 ) ) ;
#294 = EDGE_CURVE ( 'NONE', #8788, #5320, #3852, .T. ) ;
#295 = CIRCLE ( 'NONE', #9511, 17.50000000000000355 ) ;
#296 = DIRECTION ( 'NONE',  ( -0.000000000000000000, -1.000000000000000000, -0.000000000000000000 ) ) ;
#297 = CARTESIAN_POINT ( 'NONE',  ( 7.771508748547515388, 99.50000000000001421, 20.40818475981234315 ) ) ;
#298 = ORIENTED_EDGE ( 'NONE', *, *, #7410, .F. ) ;
#299 = CARTESIAN_POINT ( 'NONE',  ( 9.902568905804752575, 99.49999999999998579, 20.48863403721516363 ) ) ;
#300 = CARTESIAN_POINT ( 'NONE',  ( -11.18376618407356560, 3.249999997815050001, -27.00000000000000355 ) ) ;
#301 = CARTESIAN_POINT ( 'NONE',  ( -21.16695614262292580, 99.50000000000000000, -11.33496398805607441 ) ) ;
#302 = DIRECTION ( 'NONE',  ( -0.000000000000000000, -0.000000000000000000, -1.000000000000000000 ) ) ;
#303 = PRESENTATION_STYLE_ASSIGNMENT (( #1913 ) ) ;
#304 = CARTESIAN_POINT ( 'NONE',  ( -21.44539290152690114, 100.0000000000000000, -11.08070480119962298 ) ) ;
#305 = AXIS2_PLACEMENT_3D ( 'NONE', #9568, #7104, #7052 ) ;
#306 = PLANE ( 'NONE',  #2619 ) ;
#307 = LINE ( 'NONE', #5759, #1112 ) ;
#308 = ORIENTED_EDGE ( 'NONE', *, *, #1549, .F. ) ;
#309 = CARTESIAN_POINT ( 'NONE',  ( 5.302876193624534821E-16, -0.3375000000000000222, 2.886751345948128655 ) ) ;
#310 = EDGE_CURVE ( 'NONE', #1877, #7747, #8787, .T. ) ;
#311 = CARTESIAN_POINT ( 'NONE',  ( -2.499999999999999112, -2.662500000000000089, 1.443375672974065882 ) ) ;
#312 = CARTESIAN_POINT ( 'NONE',  ( -2.256430356250000102, -0.2906249993854829183, -1.302750673588580321 ) ) ;
#313 = CARTESIAN_POINT ( 'NONE',  ( -11.36312591709335962, 2.099999998907525089, -27.43301270000000258 ) ) ;
#314 = CARTESIAN_POINT ( 'NONE',  ( -11.18376618407358336, 0.5500000000000000444, 26.99999999999999645 ) ) ;
#315 = CARTESIAN_POINT ( 'NONE',  ( 7.826802610544922878, 99.50000000000000000, 21.21129867192371421 ) ) ;
#316 = FACE_BOUND ( 'NONE', #7653, .T. ) ;
#317 = CARTESIAN_POINT ( 'NONE',  ( 0.000000000000000000, 0.000000000000000000, 0.000000000000000000 ) ) ;
#318 = CARTESIAN_POINT ( 'NONE',  ( 8.133363296361027395, 99.50000000000004263, 19.85287606700953233 ) ) ;
#319 = EDGE_CURVE ( 'NONE', #4075, #2239, #1707, .T. ) ;
#320 = CARTESIAN_POINT ( 'NONE',  ( 3.538198506519217190, 99.99999999999998579, -24.58220198924426114 ) ) ;
#321 = CARTESIAN_POINT ( 'NONE',  ( 27.43301270000000258, 0.2499999989075251949, 0.000000000000000000 ) ) ;
#322 = EDGE_CURVE ( 'NONE', #8484, #8640, #4914, .T. ) ;
#323 = CARTESIAN_POINT ( 'NONE',  ( -2.256430356249998770, -5.165624999385483029, 1.302750673588581876 ) ) ;
#324 = LINE ( 'NONE', #3511, #9225 ) ;
#325 = CARTESIAN_POINT ( 'NONE',  ( 3.341734429721257005, 99.50000000000000000, -22.34498040423979148 ) ) ;
#326 = CARTESIAN_POINT ( 'NONE',  ( -21.52330660073277002, 100.0000000000000142, -9.647028226243550719 ) ) ;
#327 = ORIENTED_EDGE ( 'NONE', *, *, #2893, .T. ) ;
#328 = LINE ( 'NONE', #4461, #9892 ) ;
#329 = CARTESIAN_POINT ( 'NONE',  ( -1.128215178124998497, -0.6281249993854828295, 1.954126010382872147 ) ) ;
#330 = ORIENTED_EDGE ( 'NONE', *, *, #8122, .T. ) ;
#331 = CARTESIAN_POINT ( 'NONE',  ( -22.57971655928959365, 100.0000000000000000, -10.84768434062017839 ) ) ;
#332 = CARTESIAN_POINT ( 'NONE',  ( 3.739209042966563867, 99.50000000000000000, -21.42288334414699236 ) ) ;
#333 = CARTESIAN_POINT ( 'NONE',  ( 3.635130212803377781, 99.50000000000000000, -23.00575896550913768 ) ) ;
#334 = CARTESIAN_POINT ( 'NONE',  ( -15.30066472929571653, 99.99999999999998579, 16.41738810589640707 ) ) ;
#335 = ORIENTED_EDGE ( 'NONE', *, *, #10100, .T. ) ;
#336 = EDGE_LOOP ( 'NONE', ( #9504, #8678, #3054, #1608, #4599, #7689 ) ) ;
#337 = CARTESIAN_POINT ( 'NONE',  ( -16.54770463920453949, 99.99999999999998579, 15.70234036036222847 ) ) ;
#338 = CARTESIAN_POINT ( 'NONE',  ( 0.000000000000000000, -15.00000000000000000, -3.464101615137755275 ) ) ;
#339 = CARTESIAN_POINT ( 'NONE',  ( -21.86704275050744073, 100.0000000000000142, -11.06111336656620026 ) ) ;
#340 = DIRECTION ( 'NONE',  ( 0.000000000000000000, -0.000000000000000000, 1.000000000000000000 ) ) ;
#341 = VERTEX_POINT ( 'NONE', #9434 ) ;
#342 = CARTESIAN_POINT ( 'NONE',  ( -10.49999999999999822, 105.0000000000000142, 0.000000000000000000 ) ) ;
#343 = CARTESIAN_POINT ( 'NONE',  ( 11.36312591709336850, 2.599999998907525534, 27.43301269999999903 ) ) ;
#344 = DIRECTION ( 'NONE',  ( 0.000000000000000000, 0.000000000000000000, -1.000000000000000000 ) ) ;
#345 = CARTESIAN_POINT ( 'NONE',  ( 4.154273145530666511, 99.50000000000000000, -22.82723029927519676 ) ) ;
#346 = CARTESIAN_POINT ( 'NONE',  ( 7.783718120363267268, 99.49999999999998579, 21.09473326129887027 ) ) ;
#347 = CARTESIAN_POINT ( 'NONE',  ( 3.298672054714395063, 99.50000000000001421, -22.72039518595936869 ) ) ;
#348 = CARTESIAN_POINT ( 'NONE',  ( -11.18376618407358336, 5.149999997815050357, 26.99999999999999645 ) ) ;
#349 = CARTESIAN_POINT ( 'NONE',  ( 0.000000000000000000, 87.00000000000001421, -7.500000000000000000 ) ) ;
#350 =( BOUNDED_CURVE ( )  B_SPLINE_CURVE ( 2, ( #1905, #2558, #5099, #3338, #9762, #1029, #2603, #8299, #3536 ),
 .UNSPECIFIED., .F., .T. ) 
 B_SPLINE_CURVE_WITH_KNOTS ( ( 3, 2, 2, 2, 3 ),
 ( 0.8125000000000000000, 0.8194444444444444198, 0.8333333333333333703, 0.8472222222222222099, 0.8541666666666667407 ),
 .UNSPECIFIED. ) 
 CURVE ( )  GEOMETRIC_REPRESENTATION_ITEM ( )  RATIONAL_B_SPLINE_CURVE ( ( 0.9330127018922194093, 0.9330127018922194093, 1.000000000000000000, 0.8660254037844387076, 1.000000000000000000, 0.8660254037844387076, 1.000000000000000000, 0.9330127018922187432, 0.9330127018922192983 ) ) 
 REPRESENTATION_ITEM ( '' )  );
#351 = CARTESIAN_POINT ( 'NONE',  ( -21.45221949983897858, 99.50000000000000000, -9.661157428473494235 ) ) ;
#352 = DIRECTION ( 'NONE',  ( 0.000000000000000000, -1.000000000000000000, 0.000000000000000000 ) ) ;
#353 = ADVANCED_FACE ( 'NONE', ( #2833 ), #3833, .T. ) ;
#354 = CYLINDRICAL_SURFACE ( 'NONE', #9119, 2.500000000000000000 ) ;
#355 = CARTESIAN_POINT ( 'NONE',  ( 3.311778287470797721, 100.0000000000000000, -21.22295334266859967 ) ) ;
#356 = VECTOR ( 'NONE', #6599, 1000.000000000000000 ) ;
#357 = CARTESIAN_POINT ( 'NONE',  ( -2.499999999999999112, -4.856249998770965526, 1.443375672974065882 ) ) ;
#358 = VERTEX_POINT ( 'NONE', #2092 ) ;
#359 = CARTESIAN_POINT ( 'NONE',  ( 2.500000000000000000, -2.887500000000000178, -1.443375672974064994 ) ) ;
#360 = ITEM_DEFINED_TRANSFORMATION ( 'NONE', 'NONE', #9150,  #5055 ) ;
#361 = CARTESIAN_POINT ( 'NONE',  ( -14.97509118869195888, 99.99999999999997158, 15.26515554624281101 ) ) ;
#362 = CARTESIAN_POINT ( 'NONE',  ( 2.940631318607589417, 100.0000000000000000, -23.77584808773673331 ) ) ;
#363 = CARTESIAN_POINT ( 'NONE',  ( 19.39806930854668110, 2.749999998907525001, -19.39806930854668110 ) ) ;
#364 = CARTESIAN_POINT ( 'NONE',  ( -3.486133158594716510E-16, -0.5062499987709657701, -2.500000000000000000 ) ) ;
#365 = CIRCLE ( 'NONE', #10244, 2.499999999999999556 ) ;
#366 = FACE_OUTER_BOUND ( 'NONE', #5178, .T. ) ;
#367 = LINE ( 'NONE', #3559, #9996 ) ;
#368 = EDGE_CURVE ( 'NONE', #3042, #1114, #439, .T. ) ;
#369 = VERTEX_POINT ( 'NONE', #584 ) ;
#370 = CARTESIAN_POINT ( 'NONE',  ( -20.82968571475833031, 99.50000000000001421, -9.677916414284339908 ) ) ;
#371 = CARTESIAN_POINT ( 'NONE',  ( 3.028692941384139026, 100.0000000000000142, -22.52214499033115302 ) ) ;
#372 = CARTESIAN_POINT ( 'NONE',  ( 2.256430356250000102, -0.3656249993854829294, -2.763330213280484622E-16 ) ) ;
#373 = CARTESIAN_POINT ( 'NONE',  ( 11.36312591709336139, 0.3999999989075252449, -27.43301270000000258 ) ) ;
#374 =( NAMED_UNIT ( * ) SI_UNIT ( $, .STERADIAN. ) SOLID_ANGLE_UNIT ( ) );
#375 = CARTESIAN_POINT ( 'NONE',  ( 9.431378708427812896, 99.49999999999998579, 21.34379071326255684 ) ) ;
#376 = CARTESIAN_POINT ( 'NONE',  ( -7.500000000000000000, 105.0000000000000142, 1.000000000000000222 ) ) ;
#377 = ORIENTED_EDGE ( 'NONE', *, *, #7603, .T. ) ;
#378 = CARTESIAN_POINT ( 'NONE',  ( -16.18394139941567644, 99.50000000000000000, 16.57042731130403723 ) ) ;
#379 = AXIS2_PLACEMENT_3D ( 'NONE', #1311, #2259, #3050 ) ;
#380 = VECTOR ( 'NONE', #9183, 1000.000000000000000 ) ;
#381 = CARTESIAN_POINT ( 'NONE',  ( 2.256430356250000102, -0.9281249993854827629, -2.763330213280484622E-16 ) ) ;
#382 = ORIENTED_EDGE ( 'NONE', *, *, #7990, .T. ) ;
#383 = CARTESIAN_POINT ( 'NONE',  ( -22.17094027205346052, 99.99999999999998579, -9.884352203306939089 ) ) ;
#384 = FACE_OUTER_BOUND ( 'NONE', #8353, .T. ) ;
#385 = EDGE_CURVE ( 'NONE', #2107, #6279, #9699, .T. ) ;
#386 = CARTESIAN_POINT ( 'NONE',  ( -4.357666448243394824E-15, -2.137500000000000178, 2.500000000000000000 ) ) ;
#387 = CARTESIAN_POINT ( 'NONE',  ( 2.939152317953647500E-15, 73.81339255365637086, -23.99999999999999645 ) ) ;
#388 = CARTESIAN_POINT ( 'NONE',  ( 1.653273178848927064E-15, 2.600000000000000533, -27.00000000000000355 ) ) ;
#389 = ADVANCED_FACE ( 'NONE', ( #532 ), #7015, .T. ) ;
#390 = CARTESIAN_POINT ( 'NONE',  ( 4.743081672682207817, 99.50000000000002842, -21.60795120912350598 ) ) ;
#391 = FACE_OUTER_BOUND ( 'NONE', #6159, .T. ) ;
#392 = CARTESIAN_POINT ( 'NONE',  ( 3.888553205800344248, 99.49999999999995737, -24.35333287445124739 ) ) ;
#393 = VERTEX_POINT ( 'NONE', #3617 ) ;
#394 = B_SPLINE_CURVE_WITH_KNOTS ( 'NONE', 3,
 ( #7553, #5714, #8244, #9861, #7500, #8345, #4874, #1176, #4367, #3255, #8064, #8626, #6935, #2911, #8453 ),
 .UNSPECIFIED., .F., .F.,
 ( 4, 1, 1, 1, 1, 1, 1, 1, 1, 1, 1, 1, 4 ),
 ( 0.000000000000000000, 0.1101401978779246588, 0.2116695470404897084, 0.3047824012491699430, 0.3893374185178356539, 0.4648567744508144695, 0.5325800579573772842, 0.5913915682020929321, 0.6424829260185016544, 0.7344861914544180692, 0.8232371011010507500, 0.9113455750355911045, 1.000000000000000000 ),
 .UNSPECIFIED. ) ;
#395 = CARTESIAN_POINT ( 'NONE',  ( 2.204364238465235428E-15, 97.50000000000000000, -18.00000000000000000 ) ) ;
#396 = CARTESIAN_POINT ( 'NONE',  ( 19.39806930854667399, 2.649999998907525356, 19.39806930854668465 ) ) ;
#397 = CARTESIAN_POINT ( 'NONE',  ( -3.000000000000000888, -15.00000000000000000, 1.732050807568878525 ) ) ;
#398 = CARTESIAN_POINT ( 'NONE',  ( 9.838488147574068421, 99.99999999999998579, 20.25735696016189280 ) ) ;
#399 = CARTESIAN_POINT ( 'NONE',  ( 4.320351800798612807, 99.99999999999994316, -21.62386382141117736 ) ) ;
#400 = EDGE_LOOP ( 'NONE', ( #6468, #2775, #6027, #9450 ) ) ;
#401 = CARTESIAN_POINT ( 'NONE',  ( 2.912748042341355870, 99.49999999999998579, -22.34826719014139940 ) ) ;
#402 = CARTESIAN_POINT ( 'NONE',  ( 1.653273178848927064E-15, 3.199999997815050623, -27.00000000000000355 ) ) ;
#403 = PLANE ( 'NONE',  #1653 ) ;
#404 = CARTESIAN_POINT ( 'NONE',  ( -0.6698729810778054627, -0.3575961894323341772, 2.500000000000000000 ) ) ;
#405 = VERTEX_POINT ( 'NONE', #6179 ) ;
#406 = CARTESIAN_POINT ( 'NONE',  ( 4.852629679480013891, 100.0000000000000142, -23.84752007312514621 ) ) ;
#407 = AXIS2_PLACEMENT_3D ( 'NONE', #3351, #3996, #8023 ) ;
#408 = CARTESIAN_POINT ( 'NONE',  ( 11.36312591709336850, 1.799999998907525045, 27.43301269999999903 ) ) ;
#409 = EDGE_LOOP ( 'NONE', ( #1063, #2661, #6306, #7148 ) ) ;
#410 = CARTESIAN_POINT ( 'NONE',  ( -2.500000000000000000, -0.9375000000000000000, -1.443375672974064106 ) ) ;
#411 = PRODUCT_CONTEXT ( 'NONE', #6724, 'mechanical' ) ;
#412 = PLANE ( 'NONE',  #3273 ) ;
#413 = CARTESIAN_POINT ( 'NONE',  ( 4.786228327491941173E-16, -0.5906249993854828517, 2.605501347177161087 ) ) ;
#414 = CARTESIAN_POINT ( 'NONE',  ( -19.39806930854667755, 2.149999998907525356, -19.39806930854668110 ) ) ;
#415 = CARTESIAN_POINT ( 'NONE',  ( -20.42657152723830905, 100.0000000000000000, -10.54129411626120216 ) ) ;
#416 = ORIENTED_EDGE ( 'NONE', *, *, #4589, .F. ) ;
#417 = CARTESIAN_POINT ( 'NONE',  ( -15.33577160963320374, 99.99999999999998579, 16.45272793336155814 ) ) ;
#418 = LINE ( 'NONE', #2620, #6815 ) ;
#419 = DIRECTION ( 'NONE',  ( 0.2499845035238856816, 0.000000000000000000, -0.9682498375925071565 ) ) ;
#420 = AXIS2_PLACEMENT_3D ( 'NONE', #8279, #1213, #4351 ) ;
#421 = CARTESIAN_POINT ( 'NONE',  ( 3.386276725104728769, 100.0000000000000142, -24.01678749451497907 ) ) ;
#422 = CARTESIAN_POINT ( 'NONE',  ( 8.051038018032482313, 99.49999999999998579, 19.92675698219059299 ) ) ;
#423 = CARTESIAN_POINT ( 'NONE',  ( 4.820889542125314620, 99.99999999999998579, -21.76289454767624676 ) ) ;
#424 = ORIENTED_EDGE ( 'NONE', *, *, #8874, .F. ) ;
#425 = CARTESIAN_POINT ( 'NONE',  ( 2.256430356250000102, -0.8156249993854828295, -2.763330213280484622E-16 ) ) ;
#426 = CARTESIAN_POINT ( 'NONE',  ( -16.12578516900833137, 99.50000000000001421, 15.23469143358620492 ) ) ;
#427 = CARTESIAN_POINT ( 'NONE',  ( -16.38049141020750099, 100.0000000000000000, 14.97568473612765416 ) ) ;
#428 = EDGE_CURVE ( 'NONE', #5950, #1908, #2150, .T. ) ;
#429 = CARTESIAN_POINT ( 'NONE',  ( 4.061806280070601183, 99.50000000000001421, -22.51960061163626392 ) ) ;
#430 = CARTESIAN_POINT ( 'NONE',  ( 27.00000000000000355, 2.400000000000000355, 0.000000000000000000 ) ) ;
#431 = CONICAL_SURFACE ( 'NONE', #6456, 20.00000000000000000, 0.1745329251994333364 ) ;
#432 = CARTESIAN_POINT ( 'NONE',  ( 4.909381318607588973, 100.0000000000000000, -23.54377677363417121 ) ) ;
#433 = CARTESIAN_POINT ( 'NONE',  ( 2.256430356250000546, -2.315624999385482496, 1.302750673588579877 ) ) ;
#434 = ORIENTED_EDGE ( 'NONE', *, *, #1477, .F. ) ;
#435 = FACE_OUTER_BOUND ( 'NONE', #1717, .T. ) ;
#436 = CARTESIAN_POINT ( 'NONE',  ( -20.72805389903318130, 99.50000000000000000, -9.848585782927868237 ) ) ;
#437 = CARTESIAN_POINT ( 'NONE',  ( -27.00000000000000355, 4.999999997815050889, -3.306546357697854128E-15 ) ) ;
#438 = CARTESIAN_POINT ( 'NONE',  ( 4.503533123526070270, 99.49999999999995737, -24.63026223303895890 ) ) ;
#439 = B_SPLINE_CURVE_WITH_KNOTS ( 'NONE', 3,
 ( #8599, #10219, #1422, #6016, #9260, #5228, #8483, #10166, #2941, #2262, #6851, #4611, #3777, #7803, #634, #1312, #2033, #10047, #6122 ),
 .UNSPECIFIED., .F., .F.,
 ( 4, 1, 1, 1, 1, 1, 1, 1, 1, 1, 1, 1, 1, 1, 1, 1, 4 ),
 ( 0.000000000000000000, 0.06485467887857676583, 0.1277145915909605745, 0.1892127134908106190, 0.2497332716026948729, 0.3109554005383074471, 0.3726238983726959941, 0.4350931267523188151, 0.5000867325104639827, 0.5644742510850394579, 0.6276292343746815439, 0.6888483565510189477, 0.7500704854866314664, 0.8105910435985150819, 0.8724026516570742018, 0.9351453211214243444, 1.000000000000000000 ),
 .UNSPECIFIED. ) ;
#440 = AXIS2_PLACEMENT_3D ( 'NONE', #5333, #6948, #1461 ) ;
#441 = CARTESIAN_POINT ( 'NONE',  ( 4.433602057339688152, 99.50000000000000000, -21.25644978738549540 ) ) ;
#442 = CARTESIAN_POINT ( 'NONE',  ( -16.60513711880302878, 100.0000000000000000, 15.15667007515659570 ) ) ;
#443 = CYLINDRICAL_SURFACE ( 'NONE', #7131, 27.00000000000000355 ) ;
#444 = ORIENTED_EDGE ( 'NONE', *, *, #143, .F. ) ;
#445 = EDGE_CURVE ( 'NONE', #9406, #8902, #446, .T. ) ;
#446 = CIRCLE ( 'NONE', #7814, 25.00000000000000000 ) ;
#447 = CYLINDRICAL_SURFACE ( 'NONE', #8083, 27.00000000000000000 ) ;
#448 = CARTESIAN_POINT ( 'NONE',  ( 27.43301269999999548, 3.499999998907525445, 11.36312591709337738 ) ) ;
#449 = CARTESIAN_POINT ( 'NONE',  ( 5.243816414761435674, 99.50000000000000000, -23.48558366465980995 ) ) ;
#450 = ADVANCED_FACE ( 'NONE', ( #1363 ), #4557, .T. ) ;
#451 = APPLICATION_CONTEXT ( 'automotive_design' ) ;
#452 = CARTESIAN_POINT ( 'NONE',  ( 22.50000000000000355, 72.50000000000001421, -2.755455298081545172E-15 ) ) ;
#453 = STYLED_ITEM ( 'NONE', ( #5717 ), #1639 ) ;
#454 = ORIENTED_EDGE ( 'NONE', *, *, #9048, .F. ) ;
#455 = CARTESIAN_POINT ( 'NONE',  ( 9.877377282685029372E-16, -0.7312499987709657479, 2.500000000000000000 ) ) ;
#456 = CARTESIAN_POINT ( 'NONE',  ( 9.164845778125666698, 100.0000000000000142, 19.62003801130714820 ) ) ;
#457 = CARTESIAN_POINT ( 'NONE',  ( -0.6698729810778069060, -4.086153809338631149, -2.500000000000000000 ) ) ;
#458 = CARTESIAN_POINT ( 'NONE',  ( 0.000000000000000000, 100.0000000000000000, 0.000000000000000000 ) ) ;
#459 =( LENGTH_UNIT ( ) NAMED_UNIT ( * ) SI_UNIT ( .MILLI., .METRE. ) );
#460 = ORIENTED_EDGE ( 'NONE', *, *, #1580, .F. ) ;
#461 = CARTESIAN_POINT ( 'NONE',  ( -16.33590634957226229, 100.0000000000000000, 16.80570853669505382 ) ) ;
#462 = CARTESIAN_POINT ( 'NONE',  ( -19.39806930854667755, 0.6499999989075252449, -19.39806930854668110 ) ) ;
#463 = VERTEX_POINT ( 'NONE', #796 ) ;
#464 = AXIS2_PLACEMENT_3D ( 'NONE', #123, #8026, #3312 ) ;
#465 = CARTESIAN_POINT ( 'NONE',  ( -1.249999999999998224, -1.274999999999999911, 2.165063509461097713 ) ) ;
#466 = CARTESIAN_POINT ( 'NONE',  ( 0.000000000000000000, 0.000000000000000000, 0.000000000000000000 ) ) ;
#467 = CARTESIAN_POINT ( 'NONE',  ( 2.955068081869620666, 99.49999999999998579, -21.57801138750623338 ) ) ;
#468 = CARTESIAN_POINT ( 'NONE',  ( -2.256430356249999214, -2.015624999385482674, 1.302750673588581876 ) ) ;
#469 = LINE ( 'NONE', #7744, #6933 ) ;
#470 = CARTESIAN_POINT ( 'NONE',  ( 11.36312591709336850, 1.799999998907525267, 27.43301269999999903 ) ) ;
#471 = VERTEX_POINT ( 'NONE', #5661 ) ;
#472 = CARTESIAN_POINT ( 'NONE',  ( 9.263267005978743640, 99.99999999999998579, 19.65676951151765905 ) ) ;
#473 = VECTOR ( 'NONE', #4523, 1000.000000000000000 ) ;
#474 = CARTESIAN_POINT ( 'NONE',  ( 4.232798786556307036, 99.50000000000000000, -24.34936571594186105 ) ) ;
#475 = CARTESIAN_POINT ( 'NONE',  ( -4.959819536546781389E-15, 4.399999997815050357, 27.00000000000000355 ) ) ;
#476 = DIRECTION ( 'NONE',  ( 0.000000000000000000, 1.000000000000000000, 0.000000000000000000 ) ) ;
#477 = CARTESIAN_POINT ( 'NONE',  ( 1.128215178125001161, -0.4406249993854829405, 1.954126010382870815 ) ) ;
#478 = CARTESIAN_POINT ( 'NONE',  ( -1.250000000000000222, -4.124999999999999112, -2.165063509461096825 ) ) ;
#479 = ORIENTED_EDGE ( 'NONE', *, *, #7743, .T. ) ;
#480 = CARTESIAN_POINT ( 'NONE',  ( 0.6698729810778075722, -1.611153809338631282, 2.499999999999999556 ) ) ;
#481 = CARTESIAN_POINT ( 'NONE',  ( -11.36312591709335962, 1.299999998907525267, -27.43301270000000258 ) ) ;
#482 = ORIENTED_EDGE ( 'NONE', *, *, #7517, .T. ) ;
#483 = LINE ( 'NONE', #1481, #1244 ) ;
#484 = CARTESIAN_POINT ( 'NONE',  ( 9.575551604960836016, 99.99999999999994316, 20.57049984249936969 ) ) ;
#485 = CARTESIAN_POINT ( 'NONE',  ( 19.09188309203678813, 2.500000000000000000, -19.09188309203678813 ) ) ;
#486 = VERTEX_POINT ( 'NONE', #2361 ) ;
#487 = ORIENTED_EDGE ( 'NONE', *, *, #10255, .F. ) ;
#488 = CARTESIAN_POINT ( 'NONE',  ( -16.18394139941567644, 100.0000000000000000, 16.57042731130403723 ) ) ;
#489 = CARTESIAN_POINT ( 'NONE',  ( 2.256430356250000102, -2.278124999385482852, -2.763330213280484622E-16 ) ) ;
#490 = ORIENTED_EDGE ( 'NONE', *, *, #6754, .F. ) ;
#491 = ADVANCED_FACE ( 'NONE', ( #8851 ), #8702, .T. ) ;
#492 = CARTESIAN_POINT ( 'NONE',  ( 3.673940397442059178E-15, -5.000000000000000000, 30.00000000000000000 ) ) ;
#493 = CARTESIAN_POINT ( 'NONE',  ( -4.959819536546781389E-15, 3.799999999999999822, 27.00000000000000355 ) ) ;
#494 = CARTESIAN_POINT ( 'NONE',  ( 1.034219503716432668E-14, -4.556249998770965703, -2.500000000000000000 ) ) ;
#495 = B_SPLINE_SURFACE_WITH_KNOTS ( 'NONE', 3, 1, ( 
 ( #5925, #4898 ),
 ( #8143, #182 ),
 ( #1700, #1889 ),
 ( #8094, #5877 ),
 ( #6609, #8234 ),
 ( #9706, #1065 ),
 ( #5084, #6562 ),
 ( #9753, #8284 ),
 ( #5780, #5245 ),
 ( #6869, #8337 ),
 ( #4358, #6086 ),
 ( #5981, #5304 ),
 ( #8443, #2846 ),
 ( #2794, #383 ),
 ( #4518, #9278 ),
 ( #2902, #1273 ),
 ( #3576, #4464 ),
 ( #6031, #9959 ),
 ( #1167, #10065 ) ),
 .UNSPECIFIED., .F., .F., .F.,
 ( 4, 1, 1, 1, 1, 1, 1, 1, 1, 1, 1, 1, 1, 1, 1, 1, 4 ),
 ( 2, 2 ),
 ( 0.000000000000000000, 0.06441145199513656494, 0.1272798026707614161, 0.1891796676955485867, 0.2501048626594916668, 0.3106574229659737063, 0.3727353219478334867, 0.4357106927796215445, 0.5001540812204312569, 0.5646670943021733224, 0.6273118991093056263, 0.6892359343283066542, 0.7500873997029591234, 0.8110709007071082999, 0.8723115105649058565, 0.9354174373376444862, 1.000000000000000000 ),
 ( 0.000000000000000000, 1.000000000000000000 ),
 .UNSPECIFIED. ) ;
#496 = CARTESIAN_POINT ( 'NONE',  ( 2.204364238465235428E-15, 97.50000000000000000, -18.00000000000000000 ) ) ;
#497 = CARTESIAN_POINT ( 'NONE',  ( 5.142436925601051811, 99.99999999999998579, -24.04117066426968563 ) ) ;
#498 = VERTEX_POINT ( 'NONE', #3936 ) ;
#499 = CARTESIAN_POINT ( 'NONE',  ( 1.679787559701184688E-15, 5.249999998907525445, -27.43301270000000258 ) ) ;
#500 = EDGE_CURVE ( 'NONE', #7437, #3613, #793, .T. ) ;
#501 = CARTESIAN_POINT ( 'NONE',  ( -11.18376618407358336, 1.350000000000000089, 26.99999999999999645 ) ) ;
#502 = CARTESIAN_POINT ( 'NONE',  ( 4.996790860652426159E-15, -2.306249998770965259, -2.500000000000000000 ) ) ;
#503 = ORIENTED_EDGE ( 'NONE', *, *, #227, .F. ) ;
#504 = DIRECTION ( 'NONE',  ( 0.000000000000000000, 0.000000000000000000, -1.000000000000000000 ) ) ;
#505 = CARTESIAN_POINT ( 'NONE',  ( -5.039362679103552881E-15, 2.549999998907525267, 27.43301270000000258 ) ) ;
#506 = CARTESIAN_POINT ( 'NONE',  ( 2.256430356249999658, -1.228124999385483029, -1.302750673588581432 ) ) ;
#507 = DIRECTION ( 'NONE',  ( 0.2041339490496966447, 0.000000000000000000, 0.9789429660840186509 ) ) ;
#508 = ORIENTED_EDGE ( 'NONE', *, *, #6395, .T. ) ;
#509 = PLANE ( 'NONE',  #2435 ) ;
#510=STYLED_ITEM('',(#10415),#6220);
#511 = CARTESIAN_POINT ( 'NONE',  ( 10.85214315541671759, 99.50000000000000000, 22.51047735782115211 ) ) ;
#512 = EDGE_CURVE ( 'NONE', #9561, #3286, #7220, .T. ) ;
#513 = PLANE ( 'NONE',  #9858 ) ;
#514 = FACE_BOUND ( 'NONE', #4676, .T. ) ;
#515 = ORIENTED_EDGE ( 'NONE', *, *, #3140, .T. ) ;
#516 = ADVANCED_FACE ( 'NONE', ( #8750 ), #3205, .T. ) ;
#517 = CARTESIAN_POINT ( 'NONE',  ( -15.62751930918662069, 99.99999999999998579, 15.20915780906945436 ) ) ;
#518 = CARTESIAN_POINT ( 'NONE',  ( 11.36312591709336139, 1.299999998907525267, -27.43301270000000258 ) ) ;
#519 = VERTEX_POINT ( 'NONE', #3988 ) ;
#520 = CARTESIAN_POINT ( 'NONE',  ( 1.250000000000001110, -2.549999999999999822, 2.165063509461096380 ) ) ;
#521 = EDGE_CURVE ( 'NONE', #9655, #8484, #10339, .T. ) ;
#522 = PRODUCT_CONTEXT ( 'NONE', #6203, 'mechanical' ) ;
#523 = CARTESIAN_POINT ( 'NONE',  ( -22.08823018108446234, 99.50000000000000000, -9.406177930363766038 ) ) ;
#524 = CARTESIAN_POINT ( 'NONE',  ( 1.249999999999999334, -3.750000000000000000, -2.165063509461096825 ) ) ;
#525 = CARTESIAN_POINT ( 'NONE',  ( 1.128215178124999607, -0.8531249993854828073, -1.954126010382871259 ) ) ;
#526 = CARTESIAN_POINT ( 'NONE',  ( 4.901590909071964042, 99.50000000000000000, -23.62641080846013608 ) ) ;
#527 = CARTESIAN_POINT ( 'NONE',  ( -11.36312591709337383, 2.499999998907525445, 27.43301269999999548 ) ) ;
#528 = DIRECTION ( 'NONE',  ( 0.5074415416931677969, 0.000000000000000000, 0.8616861851997287269 ) ) ;
#529 = FACE_BOUND ( 'NONE', #3018, .T. ) ;
#530 = CARTESIAN_POINT ( 'NONE',  ( -16.33590634957226229, 99.50000000000000000, 16.80570853669505382 ) ) ;
#531 = EDGE_CURVE ( 'NONE', #4569, #6174, #2823, .T. ) ;
#532 = FACE_OUTER_BOUND ( 'NONE', #9383, .T. ) ;
#533 = VERTEX_POINT ( 'NONE', #1473 ) ;
#534 = CARTESIAN_POINT ( 'NONE',  ( -2.256430356250000102, -1.078124999385482896, -1.302750673588580321 ) ) ;
#535 = CARTESIAN_POINT ( 'NONE',  ( -21.71039561923405969, 99.50000000000004263, -11.44438725057713313 ) ) ;
#536 = EDGE_LOOP ( 'NONE', ( #246, #377, #3425, #10307 ) ) ;
#537 = CARTESIAN_POINT ( 'NONE',  ( 0.000000000000000000, 100.0000000000000000, -27.00000000000000355 ) ) ;
#538 = CARTESIAN_POINT ( 'NONE',  ( 27.43301270000000258, 3.449999998907525178, 0.000000000000000000 ) ) ;
#539 = SURFACE_STYLE_FILL_AREA ( #8546 ) ;
#540 = CARTESIAN_POINT ( 'NONE',  ( -15.17782247516205274, 99.99999999999994316, 15.06300032623928686 ) ) ;
#541 = CARTESIAN_POINT ( 'NONE',  ( 11.18376618407357626, 0.6500000000000001332, 27.00000000000000000 ) ) ;
#542 = CARTESIAN_POINT ( 'NONE',  ( 8.973011566395204142, 100.0000000000000000, 19.93291184930431115 ) ) ;
#543 = ORIENTED_EDGE ( 'NONE', *, *, #85, .T. ) ;
#544 = CARTESIAN_POINT ( 'NONE',  ( 4.773458297025112707, 100.0000000000000142, -24.02094923175124208 ) ) ;
#545 = CARTESIAN_POINT ( 'NONE',  ( 1.128215178125001161, -2.803124999385482319, 1.954126010382870815 ) ) ;
#546 = ORIENTED_EDGE ( 'NONE', *, *, #9397, .T. ) ;
#547 = VECTOR ( 'NONE', #4546, 1000.000000000000114 ) ;
#548 = CARTESIAN_POINT ( 'NONE',  ( 27.43301270000000258, 0.3499999989075252005, 0.000000000000000000 ) ) ;
#549 = CARTESIAN_POINT ( 'NONE',  ( -15.15193744131588183, 100.0000000000000142, 16.74589488344418697 ) ) ;
#550 = CARTESIAN_POINT ( 'NONE',  ( 8.685676809262872666, 99.50000000000000000, 23.43455588346217766 ) ) ;
#551 = CARTESIAN_POINT ( 'NONE',  ( 1.128215178124999607, -1.303124999385482985, -1.954126010382871259 ) ) ;
#552 = CARTESIAN_POINT ( 'NONE',  ( -4.959819536546781389E-15, 3.799999999999999822, 27.00000000000000355 ) ) ;
#553 = ADVANCED_FACE ( 'NONE', ( #6389 ), #3451, .F. ) ;
#554 = CARTESIAN_POINT ( 'NONE',  ( -1.767625397874844694E-16, -0.9562499987709658367, -2.886751345948128655 ) ) ;
#555 = DIRECTION ( 'NONE',  ( 0.000000000000000000, 0.000000000000000000, -1.000000000000000000 ) ) ;
#556 = FACE_OUTER_BOUND ( 'NONE', #3984, .T. ) ;
#557 = ORIENTED_EDGE ( 'NONE', *, *, #10190, .F. ) ;
#558 = CARTESIAN_POINT ( 'NONE',  ( -22.51488550592518934, 99.99999999999997158, -10.97145172607810615 ) ) ;
#559 = CARTESIAN_POINT ( 'NONE',  ( 2.500000000000000444, -4.312499999999999112, 1.443375672974063439 ) ) ;
#560 = CARTESIAN_POINT ( 'NONE',  ( -2.256430356250000102, -2.390624999385482674, 0.000000000000000000 ) ) ;
#561 = CARTESIAN_POINT ( 'NONE',  ( 9.820792995160310568, 100.0000000000000000, 20.21220011423141116 ) ) ;
#562 = EDGE_CURVE ( 'NONE', #8637, #5955, #6441, .T. ) ;
#563 = EDGE_LOOP ( 'NONE', ( #712, #7124, #2211 ) ) ;
#564 = DIRECTION ( 'NONE',  ( 0.000000000000000000, 0.000000000000000000, -1.000000000000000000 ) ) ;
#565 = CARTESIAN_POINT ( 'NONE',  ( 4.154273145530666511, 99.50000000000000000, -22.82723029927519676 ) ) ;
#566 = FACE_OUTER_BOUND ( 'NONE', #1534, .T. ) ;
#567 = ORIENTED_EDGE ( 'NONE', *, *, #4419, .F. ) ;
#568 = CARTESIAN_POINT ( 'NONE',  ( 7.500000000000000000, 104.5000000000000142, -0.9999999999999997780 ) ) ;
#569 = CARTESIAN_POINT ( 'NONE',  ( 27.43301269999999548, 1.899999998907525356, 11.36312591709337916 ) ) ;
#570 = VERTEX_POINT ( 'NONE', #7174 ) ;
#571 = CARTESIAN_POINT ( 'NONE',  ( -2.500000000000000000, -2.250000000000000000, 0.000000000000000000 ) ) ;
#572 = PRODUCT_CONTEXT ( 'NONE', #2270, 'mechanical' ) ;
#573 = CARTESIAN_POINT ( 'NONE',  ( 4.835062408351179286, 99.50000000000000000, -21.79588013901878440 ) ) ;
#574 = CARTESIAN_POINT ( 'NONE',  ( 2.864934851235464208, 99.99999999999997158, -21.80148171563692827 ) ) ;
#575 =( BOUNDED_CURVE ( )  B_SPLINE_CURVE ( 2, ( #6071, #8326, #1930, #9321, #2035, #1365, #5230 ),
 .UNSPECIFIED., .F., .F. ) 
 B_SPLINE_CURVE_WITH_KNOTS ( ( 3, 2, 2, 3 ),
 ( 0.8958333333333333703, 0.9027777777777777901, 0.9166666666666666297, 0.9258784757798345089 ),
 .UNSPECIFIED. ) 
 CURVE ( )  GEOMETRIC_REPRESENTATION_ITEM ( )  RATIONAL_B_SPLINE_CURVE ( ( 0.9330127018922192983, 0.9330127018922198534, 1.000000000000000000, 0.8660254037844387076, 1.000000000000000000, 0.9111413147426927761, 0.9401537210011674528 ) ) 
 REPRESENTATION_ITEM ( '' )  );
#576 = CARTESIAN_POINT ( 'NONE',  ( -1.595409442497313560E-16, -2.615624999385482319, -2.605501347177161087 ) ) ;
#577 = CARTESIAN_POINT ( 'NONE',  ( 1.653273178848927064E-15, 3.199999997815050623, -27.00000000000000355 ) ) ;
#578 = CARTESIAN_POINT ( 'NONE',  ( 11.36312591709336850, 3.399999998907525356, 27.43301269999999903 ) ) ;
#579 = FACE_OUTER_BOUND ( 'NONE', #8185, .T. ) ;
#580 = CIRCLE ( 'NONE', #7259, 23.99999999999999645 ) ;
#581 = CARTESIAN_POINT ( 'NONE',  ( -2.500000000000000000, -3.131249998770965881, -1.443375672974064106 ) ) ;
#582 = PLANE ( 'NONE',  #8912 ) ;
#583 = B_SPLINE_SURFACE_WITH_KNOTS ( 'NONE', 3, 1, ( 
 ( #4695, #1499 ),
 ( #4063, #7149 ),
 ( #2442, #715 ),
 ( #4743, #4640 ),
 ( #9660, #8775 ),
 ( #6419, #3963 ),
 ( #2495, #3910 ),
 ( #7833, #9609 ),
 ( #7883, #5589 ),
 ( #6263, #5689 ),
 ( #5486, #5636 ) ),
 .UNSPECIFIED., .F., .F., .F.,
 ( 4, 1, 1, 1, 1, 1, 1, 1, 4 ),
 ( 2, 2 ),
 ( 0.000000000000000000, 0.1199228846740813259, 0.2396820999030742083, 0.3587608595380448184, 0.4799620281296770319, 0.6043577515038436321, 0.7314057062717854718, 0.8632643124108332344, 1.000000000000000000 ),
 ( 0.000000000000000000, 1.000000000000000000 ),
 .UNSPECIFIED. ) ;
#584 = CARTESIAN_POINT ( 'NONE',  ( -22.57971655928959365, 99.50000000000000000, -10.84768434062017839 ) ) ;
#585 = ORIENTED_EDGE ( 'NONE', *, *, #7658, .T. ) ;
#586 = CARTESIAN_POINT ( 'NONE',  ( 2.256430356250000546, -0.4031249993854829627, 1.302750673588579877 ) ) ;
#587 = CARTESIAN_POINT ( 'NONE',  ( 0.000000000000000000, 87.00000000000001421, -25.00000000000000000 ) ) ;
#588 = ORIENTED_EDGE ( 'NONE', *, *, #9469, .F. ) ;
#589 = DIRECTION ( 'NONE',  ( -0.000000000000000000, 1.000000000000000000, -0.000000000000000000 ) ) ;
#590 = CARTESIAN_POINT ( 'NONE',  ( -27.43301270000000969, 3.899999998907524912, 11.36312591709335429 ) ) ;
#591 = LINE ( 'NONE', #8435, #9453 ) ;
#592 = EDGE_CURVE ( 'NONE', #4647, #7571, #9632, .T. ) ;
#593 = CARTESIAN_POINT ( 'NONE',  ( -19.09188309203678813, 2.100000000000000089, 19.09188309203678457 ) ) ;
#594 = DIRECTION ( 'NONE',  ( 0.000000000000000000, 0.000000000000000000, -1.000000000000000000 ) ) ;
#595 = ORIENTED_EDGE ( 'NONE', *, *, #7990, .F. ) ;
#596 = CARTESIAN_POINT ( 'NONE',  ( -19.09188309203678813, 2.900000000000000355, 19.09188309203678457 ) ) ;
#597 = CARTESIAN_POINT ( 'NONE',  ( 8.540544597724410991, 100.0000000000000000, 19.98924338346217766 ) ) ;
#598 = ORIENTED_EDGE ( 'NONE', *, *, #8582, .F. ) ;
#599 = CARTESIAN_POINT ( 'NONE',  ( -1.595409442497313560E-16, -4.865624999385482319, -2.605501347177161087 ) ) ;
#600 = VERTEX_POINT ( 'NONE', #6490 ) ;
#601 = CARTESIAN_POINT ( 'NONE',  ( -27.43301270000000258, 0.6499999989075253559, -3.359575119402369376E-15 ) ) ;
#602 = CARTESIAN_POINT ( 'NONE',  ( 0.6698729810778075722, -0.3174038105676657562, 2.499999999999999556 ) ) ;
#603 = AXIS2_PLACEMENT_3D ( 'NONE', #2574, #5908, #1150 ) ;
#604 = CARTESIAN_POINT ( 'NONE',  ( 2.256430356250000546, -1.415624999385482807, 1.302750673588579877 ) ) ;
#605 = CARTESIAN_POINT ( 'NONE',  ( 3.016803124593948393, 100.0000000000000142, -23.20507807535735978 ) ) ;
#606 = CARTESIAN_POINT ( 'NONE',  ( 4.472992770554171216, 99.99999999999995737, -21.83386288566719458 ) ) ;
#607 = CARTESIAN_POINT ( 'NONE',  ( -2.500000000000000000, -0.3937499987709658922, 0.000000000000000000 ) ) ;
#608 = CARTESIAN_POINT ( 'NONE',  ( 3.302864939465488536, 99.50000000000001421, -22.83905924565489443 ) ) ;
#609 = DIRECTION ( 'NONE',  ( 0.8660254037844384856, -0.000000000000000000, 0.5000000000000003331 ) ) ;
#610 = LINE ( 'NONE', #5438, #3877 ) ;
#611 = CARTESIAN_POINT ( 'NONE',  ( -2.256430356250000102, -1.040624999385483029, 0.000000000000000000 ) ) ;
#612 = ORIENTED_EDGE ( 'NONE', *, *, #428, .F. ) ;
#613 = DIRECTION ( 'NONE',  ( -0.000000000000000000, -0.000000000000000000, -1.000000000000000000 ) ) ;
#614 = VECTOR ( 'NONE', #3685, 1000.000000000000000 ) ;
#615 = AXIS2_PLACEMENT_3D ( 'NONE', #4071, #9758, #8930 ) ;
#616 = CARTESIAN_POINT ( 'NONE',  ( 9.263267005978743640, 99.99999999999998579, 19.65676951151765905 ) ) ;
#617 = CARTESIAN_POINT ( 'NONE',  ( -1.250000000000000222, -4.068749998770965881, -2.165063509461096825 ) ) ;
#618 = DIRECTION ( 'NONE',  ( 0.000000000000000000, -1.000000000000000000, 0.000000000000000000 ) ) ;
#619 = ORIENTED_EDGE ( 'NONE', *, *, #3800, .T. ) ;
#620 = CARTESIAN_POINT ( 'NONE',  ( -15.49723655759404295, 99.99999999999997158, 15.26389171799780264 ) ) ;
#621 = VECTOR ( 'NONE', #847, 1000.000000000000000 ) ;
#622 = CARTESIAN_POINT ( 'NONE',  ( 27.43301270000000258, 1.149999998907525356, 0.000000000000000000 ) ) ;
#623 = ORIENTED_EDGE ( 'NONE', *, *, #2893, .F. ) ;
#624 = EDGE_CURVE ( 'NONE', #3939, #7023, #5461, .T. ) ;
#625 = CARTESIAN_POINT ( 'NONE',  ( -2.500000000000000000, -4.537500000000000533, -1.443375672974064106 ) ) ;
#626 = CARTESIAN_POINT ( 'NONE',  ( 3.638175769014108774, 99.49999999999998579, -21.10017783766535970 ) ) ;
#627 = CARTESIAN_POINT ( 'NONE',  ( 1.128215178124999607, -3.103124999385482585, -1.954126010382871259 ) ) ;
#628 = CARTESIAN_POINT ( 'NONE',  ( 19.09188309203678813, 0.6999999978150504010, -19.09188309203678813 ) ) ;
#629 = CARTESIAN_POINT ( 'NONE',  ( 19.39806930854667399, 2.649999998907525356, 19.39806930854668465 ) ) ;
#630 = CARTESIAN_POINT ( 'NONE',  ( -15.91084591538827198, 100.0000000000000142, 16.65047278764667027 ) ) ;
#631 = PRODUCT_DEFINITION_FORMATION_WITH_SPECIFIED_SOURCE ( 'ANY', '', #7269, .NOT_KNOWN. ) ;
#632 = CARTESIAN_POINT ( 'NONE',  ( 4.202475441399873723, 99.50000000000000000, -24.35385978717689071 ) ) ;
#633 = CARTESIAN_POINT ( 'NONE',  ( 3.254133136943549776, 99.50000000000000000, -21.76036676155726823 ) ) ;
#634 = CARTESIAN_POINT ( 'NONE',  ( -16.18965924272485779, 99.99999999999998579, 15.26525457555968224 ) ) ;
#635 = CARTESIAN_POINT ( 'NONE',  ( -1.128215178125000273, -0.2156249993854829905, -1.954126010382871259 ) ) ;
#636 = CARTESIAN_POINT ( 'NONE',  ( -20.89052720883767122, 99.50000000000000000, -9.602653601535816819 ) ) ;
#637 = EDGE_LOOP ( 'NONE', ( #5051, #8667, #546, #8200 ) ) ;
#638 = ADVANCED_FACE ( 'NONE', ( #8160 ), #1037, .F. ) ;
#639 = ORIENTED_EDGE ( 'NONE', *, *, #3681, .F. ) ;
#640 = CARTESIAN_POINT ( 'NONE',  ( -2.256430356250000102, -2.840624999385482852, 0.000000000000000000 ) ) ;
#641 =( BOUNDED_CURVE ( )  B_SPLINE_CURVE ( 2, ( #5478, #4466, #4837, #8031, #171, #6505, #3954, #5728, #2381 ),
 .UNSPECIFIED., .F., .T. ) 
 B_SPLINE_CURVE_WITH_KNOTS ( ( 3, 2, 2, 2, 3 ),
 ( 0.6875000000000000000, 0.6944444444444444198, 0.7083333333333333703, 0.7222222222222222099, 0.7291666666666667407 ),
 .UNSPECIFIED. ) 
 CURVE ( )  GEOMETRIC_REPRESENTATION_ITEM ( )  RATIONAL_B_SPLINE_CURVE ( ( 0.9330127018922194093, 0.9330127018922194093, 1.000000000000000000, 0.8660254037844387076, 1.000000000000000000, 0.8660254037844387076, 1.000000000000000000, 0.9330127018922187432, 0.9330127018922192983 ) ) 
 REPRESENTATION_ITEM ( '' )  );
#642 = CARTESIAN_POINT ( 'NONE',  ( 11.36312591709336139, 1.999999998907525223, -27.43301270000000258 ) ) ;
#643 = LINE ( 'NONE', #2269, #10101 ) ;
#644 = CARTESIAN_POINT ( 'NONE',  ( 19.09188309203678813, 0.9000000000000001332, -19.09188309203678813 ) ) ;
#645 = AXIS2_PLACEMENT_3D ( 'NONE', #7676, #618, #5331 ) ;
#646 = CARTESIAN_POINT ( 'NONE',  ( 9.502908418173033667, 100.0000000000000284, 20.32929868008965002 ) ) ;
#647 = VERTEX_POINT ( 'NONE', #4231 ) ;
#648 = ORIENTED_EDGE ( 'NONE', *, *, #8962, .T. ) ;
#649 = CARTESIAN_POINT ( 'NONE',  ( -16.57337958714257908, 99.99999999999994316, 15.99273699073067867 ) ) ;
#650 = CARTESIAN_POINT ( 'NONE',  ( 8.281567445270807681, 100.0000000000000000, 20.15885744430370252 ) ) ;
#651 = EDGE_CURVE ( 'NONE', #7760, #2327, #205, .T. ) ;
#652 = CARTESIAN_POINT ( 'NONE',  ( 2.256430356250000546, -3.215624999385482408, 1.302750673588579877 ) ) ;
#653 = VERTEX_POINT ( 'NONE', #3345 ) ;
#654 = ORIENTED_EDGE ( 'NONE', *, *, #4623, .F. ) ;
#655 = ADVANCED_FACE ( 'NONE', ( #7411 ), #2659, .F. ) ;
#656 = CARTESIAN_POINT ( 'NONE',  ( -15.09818093130665773, 100.0000000000000000, 16.69478731934044191 ) ) ;
#657 = CARTESIAN_POINT ( 'NONE',  ( -21.08523985030068459, 99.50000000000000000, -9.874866134143449159 ) ) ;
#658 = CARTESIAN_POINT ( 'NONE',  ( -2.256430356250000102, -2.540624999385482141, -1.302750673588580321 ) ) ;
#659 = DIRECTION ( 'NONE',  ( -0.000000000000000000, 1.000000000000000000, 0.000000000000000000 ) ) ;
#660 = CARTESIAN_POINT ( 'NONE',  ( 0.000000000000000000, -15.00000000000000000, 0.000000000000000000 ) ) ;
#661 = CARTESIAN_POINT ( 'NONE',  ( 2.500000000000000000, -2.381249998770965437, -1.443375672974064994 ) ) ;
#662 = ORIENTED_EDGE ( 'NONE', *, *, #6983, .T. ) ;
#663=STYLED_ITEM('',(#10387),#6543);
#664 = DIRECTION ( 'NONE',  ( -0.000000000000000000, 1.000000000000000000, -0.000000000000000000 ) ) ;
#665 = CARTESIAN_POINT ( 'NONE',  ( 8.429066232339796017, 99.50000000000000000, 19.67794530653910101 ) ) ;
#666 = CARTESIAN_POINT ( 'NONE',  ( 1.128215178125001161, -0.8906249993854828961, 1.954126010382870815 ) ) ;
#667 = B_SPLINE_CURVE_WITH_KNOTS ( 'NONE', 3,
 ( #8704, #1525, #4822, #7964, #636, #7176, #7017, #4718, #7911, #1576, #10326, #6235, #7123, #7070, #4767, #3110, #800, #3991, #4 ),
 .UNSPECIFIED., .F., .F.,
 ( 4, 1, 1, 1, 1, 1, 1, 1, 1, 1, 1, 1, 1, 1, 1, 1, 4 ),
 ( 0.000000000000000000, 0.06358429906668214282, 0.1250797439647324816, 0.1854075229911844314, 0.2454523280917267347, 0.3052969617611028252, 0.3655926515411210831, 0.4275661794825392770, 0.4916205250740160460, 0.5555554127340263104, 0.6185525978810689773, 0.6803322039413655098, 0.7423868736098769849, 0.8044290668430417179, 0.8676072479036442964, 0.9329923078238739897, 1.000000000000000000 ),
 .UNSPECIFIED. ) ;
#668 = PRODUCT ( 'o-rings series a_iso_O-ring 45x2.65-A-ISO 3601-1', 'o-rings series a_iso_O-ring 45x2.65-A-ISO 3601-1', '', ( #10156 ) ) ;
#669 = VERTEX_POINT ( 'NONE', #158 ) ;
#670 = DIRECTION ( 'NONE',  ( 0.9415546909775123208, 0.000000000000000000, 0.3368601548094423137 ) ) ;
#671 = CARTESIAN_POINT ( 'NONE',  ( 8.751508028230254865, 99.49999999999998579, 19.58480916780017722 ) ) ;
#672 = FILL_AREA_STYLE ('',( #3972 ) ) ;
#673 = CARTESIAN_POINT ( 'NONE',  ( -22.34867803760930727, 99.49999999999998579, -10.48295844864103721 ) ) ;
#674 = ORIENTED_EDGE ( 'NONE', *, *, #7210, .F. ) ;
#675 = DIRECTION ( 'NONE',  ( 0.000000000000000000, 0.000000000000000000, 1.000000000000000000 ) ) ;
#676 = CARTESIAN_POINT ( 'NONE',  ( -19.39806930854668465, 4.849999998907525978, 19.39806930854667755 ) ) ;
#677 = EDGE_LOOP ( 'NONE', ( #674, #3279, #3413, #7812 ) ) ;
#678 = SURFACE_STYLE_FILL_AREA ( #7848 ) ;
#679 = DIRECTION ( 'NONE',  ( 0.000000000000000000, 1.000000000000000000, 0.000000000000000000 ) ) ;
#680 = CARTESIAN_POINT ( 'NONE',  ( 1.128215178124999607, -1.753124999385482718, -1.954126010382871259 ) ) ;
#681 = CARTESIAN_POINT ( 'NONE',  ( -16.91946509138130139, 99.50000000000001421, 15.98858002463268413 ) ) ;
#682 = CARTESIAN_POINT ( 'NONE',  ( -19.39806930854667755, 1.449999998907525178, -19.39806930854668110 ) ) ;
#683 = ADVANCED_FACE ( 'NONE', ( #2566 ), #4106, .T. ) ;
#684 = CARTESIAN_POINT ( 'NONE',  ( -15.30066472929571653, 99.99999999999995737, 16.41738810589640707 ) ) ;
#685 = CARTESIAN_POINT ( 'NONE',  ( 21.43339342948717885, 99.50000000000000000, -1.392427884615384803 ) ) ;
#686 = DIRECTION ( 'NONE',  ( -2.126576849575776229E-17, 0.9848077530122080203, 0.1736481776669307198 ) ) ;
#687 = DIRECTION ( 'NONE',  ( 0.000000000000000000, -1.000000000000000000, 0.000000000000000000 ) ) ;
#688 = COLOUR_RGB ( '',0.8941176470588234615, 0.8941176470588234615, 0.8941176470588234615 ) ;
#689 = CARTESIAN_POINT ( 'NONE',  ( 1.128215178124999607, -0.2906249993854829738, -1.954126010382871259 ) ) ;
#690 = CARTESIAN_POINT ( 'NONE',  ( 9.877377282685029372E-16, -3.431249998770965259, 2.500000000000000000 ) ) ;
#691 = EDGE_LOOP ( 'NONE', ( #5924, #5817, #2143, #8431 ) ) ;
#692 = ORIENTED_EDGE ( 'NONE', *, *, #9777, .F. ) ;
#693 = CARTESIAN_POINT ( 'NONE',  ( -2.256430356249999214, -1.003124999385482718, 1.302750673588581876 ) ) ;
#694 = CARTESIAN_POINT ( 'NONE',  ( 19.39806930854667399, 1.849999998907525312, 19.39806930854668465 ) ) ;
#695 = CARTESIAN_POINT ( 'NONE',  ( 1.679787559701184688E-15, 5.249999998907525445, -27.43301270000000258 ) ) ;
#696 = CARTESIAN_POINT ( 'NONE',  ( 27.00000000000000355, 2.449999999999999734, -11.18376618407356737 ) ) ;
#697 = CARTESIAN_POINT ( 'NONE',  ( 8.540544597724410991, 99.50000000000000000, 19.98924338346217766 ) ) ;
#698 = ORIENTED_EDGE ( 'NONE', *, *, #6395, .F. ) ;
#699 = EDGE_CURVE ( 'NONE', #2532, #728, #9823, .T. ) ;
#700 = CARTESIAN_POINT ( 'NONE',  ( -15.11611088805441661, 99.50000000000000000, 16.06180012866831319 ) ) ;
#701 = CARTESIAN_POINT ( 'NONE',  ( 4.154273145530666511, 100.0000000000000000, -22.82723029927519676 ) ) ;
#702 =( BOUNDED_CURVE ( )  B_SPLINE_CURVE ( 2, ( #9940, #9054, #4392, #6590, #2719, #1873, #6743, #7577, #5907 ),
 .UNSPECIFIED., .F., .T. ) 
 B_SPLINE_CURVE_WITH_KNOTS ( ( 3, 2, 2, 2, 3 ),
 ( 0.1458333333333333426, 0.1527777777777777901, 0.1666666666666666574, 0.1805555555555555525, 0.1875000000000000000 ),
 .UNSPECIFIED. ) 
 CURVE ( )  GEOMETRIC_REPRESENTATION_ITEM ( )  RATIONAL_B_SPLINE_CURVE ( ( 0.9330127018922194093, 0.9330127018922194093, 1.000000000000000000, 0.8660254037844387076, 1.000000000000000000, 0.8660254037844387076, 1.000000000000000000, 0.9330127018922194093, 0.9330127018922194093 ) ) 
 REPRESENTATION_ITEM ( '' )  );
#703 = CARTESIAN_POINT ( 'NONE',  ( -2.256430356250000102, -4.340624999385482852, -1.302750673588580321 ) ) ;
#704 = ORIENTED_EDGE ( 'NONE', *, *, #3027, .T. ) ;
#705 = ADVANCED_FACE ( 'NONE', ( #3545 ), #354, .T. ) ;
#706 = CARTESIAN_POINT ( 'NONE',  ( 11.36312591709336850, 2.499999998907525445, 27.43301269999999903 ) ) ;
#707 = CARTESIAN_POINT ( 'NONE',  ( -1.915118561403101438, -5.394273269507307234, -1.606960141313192203 ) ) ;
#708 = CARTESIAN_POINT ( 'NONE',  ( -2.256430356250000102, -1.640624999385482896, -1.302750673588580321 ) ) ;
#709 = CARTESIAN_POINT ( 'NONE',  ( 1.653273178848927064E-15, 3.400000000000000355, -27.00000000000000355 ) ) ;
#710 = FACE_OUTER_BOUND ( 'NONE', #8929, .T. ) ;
#711 = AXIS2_PLACEMENT_3D ( 'NONE', #5088, #4310, #7495 ) ;
#712 = ORIENTED_EDGE ( 'NONE', *, *, #5166, .F. ) ;
#713 = CARTESIAN_POINT ( 'NONE',  ( -2.499999999999999556, -2.156249998770965348, 1.443375672974065882 ) ) ;
#714 = ORIENTED_EDGE ( 'NONE', *, *, #1547, .T. ) ;
#715 = CARTESIAN_POINT ( 'NONE',  ( 4.693123912524271191, 100.0000000000000426, -24.12247278045041554 ) ) ;
#716 = CARTESIAN_POINT ( 'NONE',  ( -2.500000000000000000, -3.187500000000000000, -1.443375672974064106 ) ) ;
#717 = VERTEX_POINT ( 'NONE', #4175 ) ;
#718 = DIRECTION ( 'NONE',  ( 0.000000000000000000, -1.000000000000000000, 0.000000000000000000 ) ) ;
#719 = CARTESIAN_POINT ( 'NONE',  ( 1.128215178125001161, -0.4406249993854829405, 1.954126010382870815 ) ) ;
#720 = CIRCLE ( 'NONE', #4552, 2.500000000000000444 ) ;
#721 = ORIENTED_EDGE ( 'NONE', *, *, #4686, .T. ) ;
#722 = EDGE_CURVE ( 'NONE', #8554, #8603, #2756, .T. ) ;
#723 = CARTESIAN_POINT ( 'NONE',  ( -22.06741020400400188, 100.0000000000000426, -9.788922322134999021 ) ) ;
#724 = CARTESIAN_POINT ( 'NONE',  ( 9.526349065647009340, 100.0000000000000000, 19.81320455978211470 ) ) ;
#725 =( NAMED_UNIT ( * ) PLANE_ANGLE_UNIT ( ) SI_UNIT ( $, .RADIAN. ) );
#726 = PLANE ( 'NONE',  #305 ) ;
#727 = VECTOR ( 'NONE', #2964, 1000.000000000000000 ) ;
#728 = VERTEX_POINT ( 'NONE', #7314 ) ;
#729 = CARTESIAN_POINT ( 'NONE',  ( -14.89910828679519739, 99.49999999999997158, 16.44921749203638939 ) ) ;
#730 = AXIS2_PLACEMENT_3D ( 'NONE', #813, #9600, #5627 ) ;
#731 = CARTESIAN_POINT ( 'NONE',  ( -27.43301270000000969, 3.999999998907525001, 11.36312591709335784 ) ) ;
#732 = ORIENTED_EDGE ( 'NONE', *, *, #8411, .T. ) ;
#733 = CARTESIAN_POINT ( 'NONE',  ( 2.500000000000000000, -4.237499999999999822, -1.443375672974064994 ) ) ;
#734 = CARTESIAN_POINT ( 'NONE',  ( 2.843562173796539749, 99.99999999999998579, -21.91597968833000110 ) ) ;
#735 = CARTESIAN_POINT ( 'NONE',  ( 1.128215178124999607, -4.903124999385481964, -1.954126010382871259 ) ) ;
#736 = CARTESIAN_POINT ( 'NONE',  ( 0.000000000000000000, 0.000000000000000000, 0.000000000000000000 ) ) ;
#737 = CARTESIAN_POINT ( 'NONE',  ( -27.00000000000001421, 1.849999997815050534, 11.18376618407356382 ) ) ;
#738 =( GEOMETRIC_REPRESENTATION_CONTEXT ( 3 ) GLOBAL_UNCERTAINTY_ASSIGNED_CONTEXT ( ( #10215 ) ) GLOBAL_UNIT_ASSIGNED_CONTEXT ( ( #2949, #3785, #10172 ) ) REPRESENTATION_CONTEXT ( 'NONE', 'WORKASPACE' ) );
#739 = CARTESIAN_POINT ( 'NONE',  ( -15.26676860252058887, 99.99999999999995737, 16.38168943497750973 ) ) ;
#740 = FACE_OUTER_BOUND ( 'NONE', #5569, .T. ) ;
#741 = DIRECTION ( 'NONE',  ( -0.7071067811865476838, 0.000000000000000000, -0.7071067811865474617 ) ) ;
#742 = DIRECTION ( 'NONE',  ( -0.08715574274765837404, -0.9961946980917455452, 0.000000000000000000 ) ) ;
#743 = CARTESIAN_POINT ( 'NONE',  ( 4.786228327491940187E-16, -4.078124999385482674, 2.605501347177161087 ) ) ;
#744 = CARTESIAN_POINT ( 'NONE',  ( 3.207057600658871355, 100.0000000000000000, -22.07913334414698880 ) ) ;
#745 = EDGE_LOOP ( 'NONE', ( #5561, #5687, #828, #2897, #6185, #7299 ) ) ;
#746 = ADVANCED_FACE ( 'NONE', ( #9763 ), #927, .T. ) ;
#747 = CARTESIAN_POINT ( 'NONE',  ( -2.256430356249999214, -1.903124999385482852, 1.302750673588581876 ) ) ;
#748 = CARTESIAN_POINT ( 'NONE',  ( 27.43301270000000258, 4.299999998907525267, -11.36312591709336139 ) ) ;
#749 = SHAPE_REPRESENTATION_RELATIONSHIP ( 'NONE' , 'NONE' ,  #2324, #4015 ) ;
#750 = CARTESIAN_POINT ( 'NONE',  ( -15.98658610793439117, 99.50000000000001421, 14.83943845084690949 ) ) ;
#751 = CARTESIAN_POINT ( 'NONE',  ( -19.09188309203678813, 0.5000000000000000000, 19.09188309203678457 ) ) ;
#752 = FACE_OUTER_BOUND ( 'NONE', #6503, .T. ) ;
#753 = CIRCLE ( 'NONE', #7274, 23.99999999999999645 ) ;
#754 = ORIENTED_EDGE ( 'NONE', *, *, #7355, .T. ) ;
#755 = LINE ( 'NONE', #9737, #9328 ) ;
#756 = CARTESIAN_POINT ( 'NONE',  ( 8.515772100368442565, 99.50000000000000000, 20.00046577258137503 ) ) ;
#757 = CARTESIAN_POINT ( 'NONE',  ( -2.256430356250000990, -5.226765388979074167, -0.8212675591186288093 ) ) ;
#758 = PLANE ( 'NONE',  #8147 ) ;
#759 = CARTESIAN_POINT ( 'NONE',  ( 19.39806930854667399, 3.349999998907525534, 19.39806930854668465 ) ) ;
#760 = CARTESIAN_POINT ( 'NONE',  ( -19.09188309203678813, 2.100000000000000089, 19.09188309203678457 ) ) ;
#761 = ADVANCED_FACE ( 'NONE', ( #8939 ), #6178, .T. ) ;
#762 = B_SPLINE_SURFACE_WITH_KNOTS ( 'NONE', 3, 1, ( 
 ( #3955, #8033 ),
 ( #7139, #866 ),
 ( #3176, #558 ),
 ( #9555, #8085 ),
 ( #4056, #8868 ),
 ( #2383, #7240 ),
 ( #8511, #2487 ),
 ( #3317, #10137 ),
 ( #5579, #1593 ),
 ( #6507, #2536 ),
 ( #1340, #6600 ),
 ( #9063, #5917 ),
 ( #8966, #9790 ),
 ( #3461, #1783 ),
 ( #9113, #4978 ) ),
 .UNSPECIFIED., .F., .F., .F.,
 ( 4, 1, 1, 1, 1, 1, 1, 1, 1, 1, 1, 1, 4 ),
 ( 2, 2 ),
 ( 0.000000000000000000, 0.08450893420292937552, 0.1670077533940913517, 0.2489527561816328172, 0.3323249201989921797, 0.4152786837838207679, 0.4972150204155297848, 0.5791806016509544186, 0.6636863847498374325, 0.7483757861910059761, 0.8320455266939520422, 0.9153409992114193150, 1.000000000000000000 ),
 ( 0.000000000000000000, 1.000000000000000000 ),
 .UNSPECIFIED. ) ;
#763 = FACE_OUTER_BOUND ( 'NONE', #9911, .T. ) ;
#764 = CARTESIAN_POINT ( 'NONE',  ( -1.128215178125000273, -2.578124999385482674, -1.954126010382871259 ) ) ;
#765 = CARTESIAN_POINT ( 'NONE',  ( -7.500000000000000000, 104.5000000000000142, -3.000000000000000000 ) ) ;
#766 = AXIS2_PLACEMENT_3D ( 'NONE', #7049, #613, #10257 ) ;
#767 = CARTESIAN_POINT ( 'NONE',  ( -16.65546786808457469, 99.49999999999998579, 16.57295196178722918 ) ) ;
#768 = CARTESIAN_POINT ( 'NONE',  ( 9.877377282685029372E-16, -1.687499999999999778, 2.500000000000000000 ) ) ;
#769 = CARTESIAN_POINT ( 'NONE',  ( -2.499999999999999556, -3.056249998770965259, 1.443375672974065882 ) ) ;
#770 = ORIENTED_EDGE ( 'NONE', *, *, #2670, .T. ) ;
#771 = VECTOR ( 'NONE', #1661, 1000.000000000000000 ) ;
#772 = CARTESIAN_POINT ( 'NONE',  ( 0.000000000000000000, 100.0000000000000000, -27.00000000000000355 ) ) ;
#773 = CARTESIAN_POINT ( 'NONE',  ( -0.6698729810778020211, -3.242403810567665357, -2.500000000000002665 ) ) ;
#774 = FACE_OUTER_BOUND ( 'NONE', #10183, .T. ) ;
#775 = CARTESIAN_POINT ( 'NONE',  ( 1.128215178124999607, -3.440624999385482496, -1.954126010382871259 ) ) ;
#776 = VERTEX_POINT ( 'NONE', #1445 ) ;
#777 = FACE_BOUND ( 'NONE', #9157, .T. ) ;
#778 = ORIENTED_EDGE ( 'NONE', *, *, #7478, .F. ) ;
#779 = CARTESIAN_POINT ( 'NONE',  ( -22.31427554260534052, 99.50000000000002842, -10.13077409178744404 ) ) ;
#780 = EDGE_CURVE ( 'NONE', #4040, #6656, #6147, .T. ) ;
#781 = DIRECTION ( 'NONE',  ( 0.000000000000000000, 1.000000000000000000, 0.000000000000000000 ) ) ;
#782 = DIRECTION ( 'NONE',  ( -0.000000000000000000, 1.000000000000000000, -0.000000000000000000 ) ) ;
#783 = ORIENTED_EDGE ( 'NONE', *, *, #1218, .F. ) ;
#784 = ADVANCED_FACE ( 'NONE', ( #710 ), #3851, .T. ) ;
#785 = CARTESIAN_POINT ( 'NONE',  ( -1.345399338949505808, -5.026709289312093709, -2.285932919781461958 ) ) ;
#786 = VECTOR ( 'NONE', #10019, 1000.000000000000114 ) ;
#787 = CARTESIAN_POINT ( 'NONE',  ( 3.212364564527730337, 100.0000000000000000, -22.10366694310577884 ) ) ;
#788 = CARTESIAN_POINT ( 'NONE',  ( -1.595409442497313560E-16, -4.415624999385482141, -2.605501347177161087 ) ) ;
#789 = CARTESIAN_POINT ( 'NONE',  ( -20.99557965837879081, 99.49999999999997158, -10.74478602187354959 ) ) ;
#790 = CARTESIAN_POINT ( 'NONE',  ( -19.39806930854668465, 4.049999998907525267, 19.39806930854667755 ) ) ;
#791 = UNCERTAINTY_MEASURE_WITH_UNIT (LENGTH_MEASURE( 1.000000000000000082E-05 ), #10331, 'distance_accuracy_value', 'NONE');
#792 = CARTESIAN_POINT ( 'NONE',  ( -20.63666786535793207, 99.49999999999998579, -10.16306733409737717 ) ) ;
#793 = CIRCLE ( 'NONE', #3298, 1.324999999999999734 ) ;
#794 = LINE ( 'NONE', #1520, #8161 ) ;
#795 = CARTESIAN_POINT ( 'NONE',  ( -15.31787750341841559, 99.50000000000001421, 16.43551622900274722 ) ) ;
#796 = CARTESIAN_POINT ( 'NONE',  ( 10.85214315541671759, 100.0000000000000000, 22.51047735782115211 ) ) ;
#797 = AXIS2_PLACEMENT_3D ( 'NONE', #9860, #6717, #4315 ) ;
#798 =( GEOMETRIC_REPRESENTATION_CONTEXT ( 3 ) GLOBAL_UNCERTAINTY_ASSIGNED_CONTEXT ( ( #8646 ) ) GLOBAL_UNIT_ASSIGNED_CONTEXT ( ( #7893, #725, #8735 ) ) REPRESENTATION_CONTEXT ( 'NONE', 'WORKASPACE' ) );
#799 = CARTESIAN_POINT ( 'NONE',  ( -1.595409442497313560E-16, -3.853124999385482585, -2.605501347177161087 ) ) ;
#800 = CARTESIAN_POINT ( 'NONE',  ( -21.99154324187120579, 99.50000000000001421, -9.362771248264911250 ) ) ;
#801 = CARTESIAN_POINT ( 'NONE',  ( 2.256430356250000546, -2.203124999385482674, 1.302750673588579877 ) ) ;
#802 = CARTESIAN_POINT ( 'NONE',  ( -11.36312591709337383, 1.699999998907525178, 27.43301269999999548 ) ) ;
#803 = CARTESIAN_POINT ( 'NONE',  ( 1.679787559701184688E-15, 5.316666665574192763, -27.43301270000000258 ) ) ;
#804 = CARTESIAN_POINT ( 'NONE',  ( 19.09188309203678813, 3.299999999999999822, -19.09188309203678813 ) ) ;
#805 = CARTESIAN_POINT ( 'NONE',  ( 2.964854786877021642, 100.0000000000000000, -22.43901021186594846 ) ) ;
#806 = CARTESIAN_POINT ( 'NONE',  ( -2.256430356250000102, -0.1406249993854829794, 0.000000000000000000 ) ) ;
#807 = CARTESIAN_POINT ( 'NONE',  ( 8.187169943530866689, 99.49999999999998579, 20.27434297626003712 ) ) ;
#808 = ORIENTED_EDGE ( 'NONE', *, *, #8492, .T. ) ;
#809 = CARTESIAN_POINT ( 'NONE',  ( 0.000000000000000000, 0.000000000000000000, 0.000000000000000000 ) ) ;
#810 = ORIENTED_EDGE ( 'NONE', *, *, #9, .F. ) ;
#811 = CARTESIAN_POINT ( 'NONE',  ( 11.36312591709336139, 3.599999998907525089, -27.43301270000000258 ) ) ;
#812 = CARTESIAN_POINT ( 'NONE',  ( 3.977571997893210032, 100.0000000000000000, -24.70179182097838932 ) ) ;
#813 = CARTESIAN_POINT ( 'NONE',  ( 9.248677610544923766, 99.50000000000000000, 22.83089001807756446 ) ) ;
#814 = AXIS2_PLACEMENT_3D ( 'NONE', #8760, #6354, #2424 ) ;
#815 = CARTESIAN_POINT ( 'NONE',  ( 2.256430356249999658, -4.490624999385482319, -1.302750673588581432 ) ) ;
#816 = DIRECTION ( 'NONE',  ( 0.000000000000000000, 1.000000000000000000, 0.000000000000000000 ) ) ;
#817 = CARTESIAN_POINT ( 'NONE',  ( -4.959819536546781389E-15, 1.399999999999999911, 27.00000000000000355 ) ) ;
#818 = CARTESIAN_POINT ( 'NONE',  ( 11.18376618407357626, 5.249999997815050889, 27.00000000000000000 ) ) ;
#819 = ORIENTED_EDGE ( 'NONE', *, *, #5028, .T. ) ;
#820 = EDGE_CURVE ( 'NONE', #224, #4694, #7051, .T. ) ;
#821 = AXIS2_PLACEMENT_3D ( 'NONE', #7498, #239, #4948 ) ;
#822 = CARTESIAN_POINT ( 'NONE',  ( 2.500000000000000000, -1.481249998770965970, -1.443375672974064994 ) ) ;
#823 = FACE_OUTER_BOUND ( 'NONE', #7757, .T. ) ;
#824 = DIRECTION ( 'NONE',  ( 0.000000000000000000, 0.000000000000000000, -1.000000000000000000 ) ) ;
#825 = CARTESIAN_POINT ( 'NONE',  ( -21.30928386698190025, 99.50000000000000000, -11.02857376369709996 ) ) ;
#826 = CARTESIAN_POINT ( 'NONE',  ( 2.256430356250000102, -4.415624999385482141, -2.763330213280484622E-16 ) ) ;
#827 = VERTEX_POINT ( 'NONE', #4374 ) ;
#828 = ORIENTED_EDGE ( 'NONE', *, *, #7593, .T. ) ;
#829 = CARTESIAN_POINT ( 'NONE',  ( 0.000000000000000000, -25.00000000000000000, -2.062556682370379590 ) ) ;
#830 = CARTESIAN_POINT ( 'NONE',  ( 0.000000000000000000, 0.000000000000000000, 0.000000000000000000 ) ) ;
#831 = CARTESIAN_POINT ( 'NONE',  ( -22.35642768247353729, 99.49999999999995737, -10.34293228154892752 ) ) ;
#832 = CARTESIAN_POINT ( 'NONE',  ( -14.97509118869195888, 99.49999999999998579, 15.26515554624281101 ) ) ;
#833 = CARTESIAN_POINT ( 'NONE',  ( -5.039362679103552881E-15, 4.149999998907524912, 27.43301270000000258 ) ) ;
#834 = VERTEX_POINT ( 'NONE', #9345 ) ;
#835 = CARTESIAN_POINT ( 'NONE',  ( -1.249999999999998224, -4.875000000000000000, 2.165063509461097713 ) ) ;
#836 = ITEM_DEFINED_TRANSFORMATION ( 'NONE', 'NONE', #9499,  #5055 ) ;
#837 = CARTESIAN_POINT ( 'NONE',  ( -20.96129225301843135, 100.0000000000000142, -10.68089388303413934 ) ) ;
#838 = CARTESIAN_POINT ( 'NONE',  ( -1.128215178125000273, -3.928124999385483207, -1.954126010382871259 ) ) ;
#839 = EDGE_CURVE ( 'NONE', #1713, #9182, #7041, .T. ) ;
#840 = CARTESIAN_POINT ( 'NONE',  ( -21.13504512532655610, 99.50000000000000000, -11.31853095674525100 ) ) ;
#841 = CARTESIAN_POINT ( 'NONE',  ( -11.36312591709337383, 4.099999998907525089, 27.43301269999999548 ) ) ;
#842 = CARTESIAN_POINT ( 'NONE',  ( -15.26676860252058887, 99.49999999999998579, 16.38168943497750973 ) ) ;
#843 = EDGE_CURVE ( 'NONE', #1838, #1383, #2583, .T. ) ;
#844 = CARTESIAN_POINT ( 'NONE',  ( 0.000000000000000000, 0.000000000000000000, 0.000000000000000000 ) ) ;
#845 = CARTESIAN_POINT ( 'NONE',  ( 3.231466532446834350, 99.99999999999997158, -21.81145066552309686 ) ) ;
#846 = PRODUCT_DEFINITION_SHAPE ( 'NONE', 'NONE',  #4215 ) ;
#847 = DIRECTION ( 'NONE',  ( 0.000000000000000000, -1.000000000000000000, 0.000000000000000000 ) ) ;
#848 = CARTESIAN_POINT ( 'NONE',  ( 1.128215178124999607, -3.440624999385482496, -1.954126010382871259 ) ) ;
#849 = CARTESIAN_POINT ( 'NONE',  ( 9.820792995160308791, 100.0000000000000000, 20.21220011423140761 ) ) ;
#850 = ADVANCED_FACE ( 'NONE', ( #5431, #7830 ), #2335, .F. ) ;
#851 = EDGE_LOOP ( 'NONE', ( #9977, #8377 ) ) ;
#852 = CARTESIAN_POINT ( 'NONE',  ( 2.256430356250000102, -2.615624999385482763, -2.763330213280484622E-16 ) ) ;
#853 = CARTESIAN_POINT ( 'NONE',  ( -11.36312591709335962, 4.499999998907525445, -27.43301270000000258 ) ) ;
#854 = DIRECTION ( 'NONE',  ( -0.1697592580069431922, 0.000000000000000000, 0.9854855627156250408 ) ) ;
#855 = CARTESIAN_POINT ( 'NONE',  ( -5.039362679103552881E-15, 0.8499999989075253115, 27.43301270000000258 ) ) ;
#856 = CARTESIAN_POINT ( 'NONE',  ( 1.034219503716432668E-14, -3.206249998770966059, -2.500000000000000000 ) ) ;
#857 = ORIENTED_EDGE ( 'NONE', *, *, #9277, .F. ) ;
#858 = EDGE_CURVE ( 'NONE', #7847, #7747, #5465, .T. ) ;
#859 =( BOUNDED_CURVE ( )  B_SPLINE_CURVE ( 2, ( #959, #2579, #170, #5072, #8963, #4976, #4196, #480, #6128 ),
 .UNSPECIFIED., .F., .F. ) 
 B_SPLINE_CURVE_WITH_KNOTS ( ( 3, 2, 2, 2, 3 ),
 ( 0.1875000000000000000, 0.1944444444444444475, 0.2083333333333333426, 0.2222222222222222099, 0.2291666666666666574 ),
 .UNSPECIFIED. ) 
 CURVE ( )  GEOMETRIC_REPRESENTATION_ITEM ( )  RATIONAL_B_SPLINE_CURVE ( ( 0.9330127018922194093, 0.9330127018922194093, 1.000000000000000000, 0.8660254037844387076, 1.000000000000000000, 0.8660254037844387076, 1.000000000000000000, 0.9330127018922194093, 0.9330127018922194093 ) ) 
 REPRESENTATION_ITEM ( '' )  );
#860 = CARTESIAN_POINT ( 'NONE',  ( 8.132491713109025966, 99.50000000000000000, 21.08089001807756091 ) ) ;
#861 = CARTESIAN_POINT ( 'NONE',  ( 4.909381318607588973, 99.50000000000000000, -23.54377677363417121 ) ) ;
#862 = ORIENTED_EDGE ( 'NONE', *, *, #2814, .T. ) ;
#863 = CARTESIAN_POINT ( 'NONE',  ( -11.36312591709337561, 3.999999998907525889, 27.43301269999999548 ) ) ;
#864 = LINE ( 'NONE', #8915, #7733 ) ;
#865 = APPLICATION_CONTEXT ( 'automotive_design' ) ;
#866 = CARTESIAN_POINT ( 'NONE',  ( -22.55793349878803156, 100.0000000000000000, -10.88926985104519929 ) ) ;
#867 = CARTESIAN_POINT ( 'NONE',  ( 1.128215178125001161, -5.053124999385482319, 1.954126010382870815 ) ) ;
#868 = CARTESIAN_POINT ( 'NONE',  ( -16.54770463920453949, 100.0000000000000284, 15.70234036036222847 ) ) ;
#869 = CARTESIAN_POINT ( 'NONE',  ( -16.84090648038580085, 99.99999999999998579, 15.49469789757679727 ) ) ;
#870 = CARTESIAN_POINT ( 'NONE',  ( 5.142436925601051811, 99.99999999999995737, -24.04117066426968563 ) ) ;
#871 = CARTESIAN_POINT ( 'NONE',  ( -1.249999999999998224, -2.568749998770965437, 2.165063509461097713 ) ) ;
#872 = VERTEX_POINT ( 'NONE', #5374 ) ;
#873 = CARTESIAN_POINT ( 'NONE',  ( 8.685676809262872666, 99.50000000000000000, 23.43455588346217766 ) ) ;
#874 = EDGE_CURVE ( 'NONE', #3238, #9838, #4617, .T. ) ;
#875 = CARTESIAN_POINT ( 'NONE',  ( -14.83571502646304197, 100.0000000000000426, 16.32397075880403392 ) ) ;
#876 = CARTESIAN_POINT ( 'NONE',  ( -2.256430356249999214, -3.703124999385482674, 1.302750673588581876 ) ) ;
#877 = AXIS2_PLACEMENT_3D ( 'NONE', #9689, #1582, #14 ) ;
#878 = ORIENTED_EDGE ( 'NONE', *, *, #6262, .F. ) ;
#879 = DIRECTION ( 'NONE',  ( 0.3368601548094422582, 0.000000000000000000, -0.9415546909775122097 ) ) ;
#880 = DIRECTION ( 'NONE',  ( 0.000000000000000000, -1.000000000000000000, 0.000000000000000000 ) ) ;
#881 = CARTESIAN_POINT ( 'NONE',  ( -22.28738277804067636, 99.49999999999997158, -10.06255608345902886 ) ) ;
#882 = DIRECTION ( 'NONE',  ( -0.000000000000000000, -1.000000000000000000, -0.000000000000000000 ) ) ;
#883 = VECTOR ( 'NONE', #5087, 1000.000000000000114 ) ;
#884 = CARTESIAN_POINT ( 'NONE',  ( 9.482997300390421103, 100.0000000000000000, 20.28643943712827991 ) ) ;
#885 = AXIS2_PLACEMENT_3D ( 'NONE', #1301, #7484, #4250 ) ;
#886 = FACE_OUTER_BOUND ( 'NONE', #8707, .T. ) ;
#887 = EDGE_CURVE ( 'NONE', #1976, #26, #7608, .T. ) ;
#888 = CARTESIAN_POINT ( 'NONE',  ( 3.269123371500344710, 99.99999999999998579, -23.64665713169964434 ) ) ;
#889 = CARTESIAN_POINT ( 'NONE',  ( -1.128215178124998497, -5.128124999385482496, 1.954126010382872147 ) ) ;
#890 = CARTESIAN_POINT ( 'NONE',  ( -21.24310748994415832, 99.49999999999998579, -10.99527971241054658 ) ) ;
#891 = CARTESIAN_POINT ( 'NONE',  ( -5.039362679103552881E-15, 4.949999998907525622, 27.43301270000000258 ) ) ;
#892 = CARTESIAN_POINT ( 'NONE',  ( -15.15623813234777018, 99.50000000000000000, 16.19783826294960249 ) ) ;
#893 = AXIS2_PLACEMENT_3D ( 'NONE', #8051, #4077, #5944 ) ;
#894 = CARTESIAN_POINT ( 'NONE',  ( -21.94169572595625795, 100.0000000000000000, -9.715372641902229489 ) ) ;
#895 = CARTESIAN_POINT ( 'NONE',  ( -15.55395551812965671, 99.50000000000002842, 16.59868653893595791 ) ) ;
#896 = CARTESIAN_POINT ( 'NONE',  ( -22.51767453479306980, 100.0000000000000000, -9.764155749770198511 ) ) ;
#897 = CARTESIAN_POINT ( 'NONE',  ( 2.256430356250000546, -3.553124999385482763, 1.302750673588579877 ) ) ;
#898 = PLANE ( 'NONE',  #9130 ) ;
#899 = CARTESIAN_POINT ( 'NONE',  ( 2.256430356250000546, -4.453124999385482674, 1.302750673588579877 ) ) ;
#900 = CARTESIAN_POINT ( 'NONE',  ( 11.36312591709336139, 4.399999998907525800, -27.43301270000000258 ) ) ;
#901 = SHAPE_REPRESENTATION_RELATIONSHIP ( 'NONE' , 'NONE' ,  #177, #3150 ) ;
#902 = CARTESIAN_POINT ( 'NONE',  ( -16.07368679829020763, 99.50000000000000000, 17.11560437002838952 ) ) ;
#903 = STYLED_ITEM ( 'NONE', ( #2100 ), #7366 ) ;
#904 = CARTESIAN_POINT ( 'NONE',  ( -4.959819536546781389E-15, 4.599999999999999645, 27.00000000000000355 ) ) ;
#905 = CARTESIAN_POINT ( 'NONE',  ( -20.79740905086423552, 100.0000000000000142, -11.06234285579171051 ) ) ;
#906 = VERTEX_POINT ( 'NONE', #10349 ) ;
#907 = CARTESIAN_POINT ( 'NONE',  ( -16.35834224700816009, 99.50000000000000000, 16.43761959438736397 ) ) ;
#908 = DIRECTION ( 'NONE',  ( -0.000000000000000000, -1.000000000000000000, -0.000000000000000000 ) ) ;
#909 = ORIENTED_EDGE ( 'NONE', *, *, #1596, .F. ) ;
#910 = CARTESIAN_POINT ( 'NONE',  ( -20.77412980915959650, 99.49999999999997158, -9.759484723497815040 ) ) ;
#911 = EDGE_CURVE ( 'NONE', #9838, #3238, #8959, .T. ) ;
#912 = DIRECTION ( 'NONE',  ( -0.9415543565890244215, 0.000000000000000000, -0.3368610894541372303 ) ) ;
#913 = CARTESIAN_POINT ( 'NONE',  ( 3.409892249890944527, 100.0000000000000000, -24.50637943905448779 ) ) ;
#914 = EDGE_CURVE ( 'NONE', #3286, #6080, #4178, .T. ) ;
#915 = CARTESIAN_POINT ( 'NONE',  ( -19.09188309203678457, 0.8999999978150503566, -19.09188309203678813 ) ) ;
#916 = CARTESIAN_POINT ( 'NONE',  ( 2.256430356250000546, -5.015624999385481786, 1.302750673588579877 ) ) ;
#917 = CARTESIAN_POINT ( 'NONE',  ( -16.37547766376588854, 100.0000000000000000, 16.41943072543956816 ) ) ;
#918 = CARTESIAN_POINT ( 'NONE',  ( -22.13144646319157260, 100.0000000000000142, -9.428651666388001118 ) ) ;
#919 = CARTESIAN_POINT ( 'NONE',  ( 8.081885929396888102, 100.0000000000000142, 20.89785832093561169 ) ) ;
#920 =( BOUNDED_CURVE ( )  B_SPLINE_CURVE ( 2, ( #8344, #2554, #4366, #6572, #1021, #8932, #147, #3529, #4218 ),
 .UNSPECIFIED., .F., .T. ) 
 B_SPLINE_CURVE_WITH_KNOTS ( ( 3, 2, 2, 2, 3 ),
 ( 0.6041666666666667407, 0.6111111111111111605, 0.6250000000000000000, 0.6388888888888888395, 0.6458333333333333703 ),
 .UNSPECIFIED. ) 
 CURVE ( )  GEOMETRIC_REPRESENTATION_ITEM ( )  RATIONAL_B_SPLINE_CURVE ( ( 0.9330127018922192983, 0.9330127018922198534, 1.000000000000000000, 0.8660254037844387076, 1.000000000000000000, 0.8660254037844387076, 1.000000000000000000, 0.9330127018922187432, 0.9330127018922192983 ) ) 
 REPRESENTATION_ITEM ( '' )  );
#921 = CARTESIAN_POINT ( 'NONE',  ( 2.500000000000000000, -4.631249998770965881, -1.443375672974064994 ) ) ;
#922 = ORIENTED_EDGE ( 'NONE', *, *, #4166, .T. ) ;
#923 = CYLINDRICAL_SURFACE ( 'NONE', #5111, 2.500000000000000000 ) ;
#924 = CARTESIAN_POINT ( 'NONE',  ( -15.58193289918752278, 100.0000000000000000, 16.98546238400348329 ) ) ;
#925 = CARTESIAN_POINT ( 'NONE',  ( 9.184850993605147944E-16, 87.00000000000001421, 7.500000000000000000 ) ) ;
#926 = CARTESIAN_POINT ( 'NONE',  ( 1.128215178125001161, -4.040624999385483029, 1.954126010382870815 ) ) ;
#927 = B_SPLINE_SURFACE_WITH_KNOTS ( 'NONE', 3, 1, ( 
 ( #8251, #3487 ),
 ( #5795, #3339 ),
 ( #346, #8300 ),
 ( #5100, #9089 ),
 ( #245, #8987 ),
 ( #2559, #6671 ),
 ( #3429, #9867 ),
 ( #2652, #1807 ),
 ( #297, #5154 ),
 ( #1078, #6726 ),
 ( #152, #7456 ),
 ( #3537, #7507 ),
 ( #6623, #1959 ),
 ( #5893, #6530 ),
 ( #1906, #9922 ),
 ( #5948, #4223 ),
 ( #4130, #4274 ),
 ( #7403, #3380 ),
 ( #6575, #2604 ) ),
 .UNSPECIFIED., .F., .F., .F.,
 ( 4, 1, 1, 1, 1, 1, 1, 1, 1, 1, 1, 1, 1, 1, 1, 1, 4 ),
 ( 2, 2 ),
 ( 0.000000000000000000, 0.06839333837245492598, 0.1346519561570838353, 0.1985335841112251809, 0.2613354512981445610, 0.3228799447584090876, 0.3842093944964607433, 0.4462111754260434937, 0.5089246482083435996, 0.5715029624870164859, 0.6324491702983550123, 0.6923675070709934820, 0.7521785462597534444, 0.8119602890481165680, 0.8728645645504365946, 0.9355733815441056311, 1.000000000000000000 ),
 ( 0.000000000000000000, 1.000000000000000000 ),
 .UNSPECIFIED. ) ;
#928 = ORIENTED_EDGE ( 'NONE', *, *, #3384, .F. ) ;
#929 = AXIS2_PLACEMENT_3D ( 'NONE', #6755, #5824, #3568 ) ;
#930 = CARTESIAN_POINT ( 'NONE',  ( -20.63200021313574695, 99.50000000000000000, -10.19493994959453431 ) ) ;
#931 = LINE ( 'NONE', #8151, #4479 ) ;
#932 = CARTESIAN_POINT ( 'NONE',  ( -15.07178375341841559, 99.50000000000001421, 15.16157792772069968 ) ) ;
#933 = CARTESIAN_POINT ( 'NONE',  ( -27.00000000000001421, 4.450000000000000178, 11.18376618407356560 ) ) ;
#934 = EDGE_LOOP ( 'NONE', ( #1052, #10025 ) ) ;
#935 = DIRECTION ( 'NONE',  ( 0.000000000000000000, 0.000000000000000000, -1.000000000000000000 ) ) ;
#936 = CARTESIAN_POINT ( 'NONE',  ( 4.061806280070601183, 100.0000000000000142, -22.51960061163626392 ) ) ;
#937 = CARTESIAN_POINT ( 'NONE',  ( 4.232447118646125439, 99.49999999999998579, -21.54138831197867887 ) ) ;
#938 = CARTESIAN_POINT ( 'NONE',  ( -20.91264567078791714, 99.49999999999997158, -10.54226115003387676 ) ) ;
#939 = CARTESIAN_POINT ( 'NONE',  ( -27.43301270000000969, 3.999999998907525001, 11.36312591709335429 ) ) ;
#940 = CIRCLE ( 'NONE', #3608, 27.00000000000000000 ) ;
#941 = CARTESIAN_POINT ( 'NONE',  ( -4.959819536546781389E-15, 3.000000000000000000, 27.00000000000000355 ) ) ;
#942 = CARTESIAN_POINT ( 'NONE',  ( 11.18376618407357093, 3.949999997815050179, -27.00000000000000355 ) ) ;
#943 = CARTESIAN_POINT ( 'NONE',  ( -15.83671465916681242, 99.50000000000000000, 16.65403364262263608 ) ) ;
#944 = ADVANCED_FACE ( 'NONE', ( #24 ), #4011, .F. ) ;
#945 = CARTESIAN_POINT ( 'NONE',  ( -21.37606745505193473, 99.50000000000002842, -11.05925878703054011 ) ) ;
#946 = CARTESIAN_POINT ( 'NONE',  ( -2.256430356249998770, -4.153124999385482852, 1.302750673588581876 ) ) ;
#947 = ORIENTED_EDGE ( 'NONE', *, *, #3571, .F. ) ;
#948 = CARTESIAN_POINT ( 'NONE',  ( -1.595409442497313560E-16, -3.403124999385483296, -2.605501347177161087 ) ) ;
#949 = FACE_OUTER_BOUND ( 'NONE', #8574, .T. ) ;
#950 = CARTESIAN_POINT ( 'NONE',  ( 27.43301269999999548, 0.9999999989075254447, 11.36312591709337738 ) ) ;
#951 = B_SPLINE_CURVE_WITH_KNOTS ( 'NONE', 3,
 ( #8897, #7961, #5660, #4036, #2412, #6536, #7173, #3986, #9723, #943, #10366, #4137, #3344, #895, #7319, #5607, #108, #3251, #795 ),
 .UNSPECIFIED., .F., .F.,
 ( 4, 1, 1, 1, 1, 1, 1, 1, 1, 1, 1, 1, 1, 1, 1, 1, 4 ),
 ( 0.000000000000000000, 0.06473117683888822416, 0.1283191082976379849, 0.1900130092022370987, 0.2509653124206144836, 0.3118694605430146760, 0.3735603890354366463, 0.4359106579620777855, 0.5007804971236301528, 0.5656503362851855732, 0.6280858374182423098, 0.6899222460797727052, 0.7510277903999277305, 0.8114330998898260372, 0.8726106248506092511, 0.9357151229638154266, 1.000000000000000000 ),
 .UNSPECIFIED. ) ;
#952 = DIRECTION ( 'NONE',  ( 0.000000000000000000, 0.000000000000000000, -1.000000000000000000 ) ) ;
#953 = DIRECTION ( 'NONE',  ( 1.000000000000000000, 0.000000000000000000, 0.000000000000000000 ) ) ;
#954 = CIRCLE ( 'NONE', #7972, 30.00000000000000000 ) ;
#955 = LINE ( 'NONE', #7185, #3544 ) ;
#956 = EDGE_CURVE ( 'NONE', #4002, #7760, #7549, .T. ) ;
#957 = VERTEX_POINT ( 'NONE', #3323 ) ;
#958 = AXIS2_PLACEMENT_3D ( 'NONE', #6633, #9875, #3391 ) ;
#959 = CARTESIAN_POINT ( 'NONE',  ( -3.486133158594716510E-16, -1.406249998770965570, -2.500000000000000000 ) ) ;
#960 = DIRECTION ( 'NONE',  ( -0.000000000000000000, -1.000000000000000000, -0.000000000000000000 ) ) ;
#961 = SURFACE_STYLE_FILL_AREA ( #5129 ) ;
#962 = CARTESIAN_POINT ( 'NONE',  ( -2.256430356249998770, -3.815624999385482941, 1.302750673588581876 ) ) ;
#963 = LINE ( 'NONE', #3178, #4889 ) ;
#964 = CARTESIAN_POINT ( 'NONE',  ( -16.90689012439429462, 99.49999999999998579, 16.08742389234230785 ) ) ;
#965 = CARTESIAN_POINT ( 'NONE',  ( 5.207032889226773875, 100.0000000000000000, -23.83708953234284778 ) ) ;
#966 = EDGE_CURVE ( 'NONE', #2239, #2880, #5183, .T. ) ;
#967 = EDGE_CURVE ( 'NONE', #7282, #872, #8454, .T. ) ;
#968 = CARTESIAN_POINT ( 'NONE',  ( 2.500000000000000444, -5.156249998770965348, 1.443375672974063439 ) ) ;
#969 = VERTEX_POINT ( 'NONE', #8920 ) ;
#970 = ORIENTED_EDGE ( 'NONE', *, *, #3832, .F. ) ;
#971 = DIRECTION ( 'NONE',  ( 0.000000000000000000, -1.000000000000000000, 0.000000000000000000 ) ) ;
#972 = FACE_OUTER_BOUND ( 'NONE', #7578, .T. ) ;
#973 = CARTESIAN_POINT ( 'NONE',  ( -21.37606745505193473, 99.50000000000002842, -11.05925878703054011 ) ) ;
#974 =( BOUNDED_CURVE ( )  B_SPLINE_CURVE ( 2, ( #9222, #7089, #10068, #5429, #4578, #10240, #10294, #2227, #2112, #8722, #4521, #9456, #7714, #1386, #9281, #8618, #6314, #2966, #3849, #2905, #5480, #1442, #7773, #3073, #3126, #4635, #5309, #1542, #551, #2282, #3744, #604, #8504, #7828, #9508, #3901, #3024, #708, #4736, #3802, #6985, #1334, #6927, #10128, #8671, #10187, #6872, #1494, #6200, #6256, #9398, #6145, #9343, #2332, #6089, #2172, #5371, #8561, #4690, #5531, #7930, #658, #764, #7038, #7875, #5580, #2581, #6362, #8869, #4057, #9745, #5774, #4786, #6463, #3956, #4107, #21, #8768, #1784, #3319, #7193, #5731, #9650, #2537, #7983, #5681, #8819, #9556, #6508, #8178, #4980, #7291, #8967, #2384, #3177, #962, #1648, #8917, #1738, #7241, #2488, #3224, #9697, #3361, #1594, #7141, #4935, #6554, #130, #4839, #10346, #4008, #8133, #815, #1694, #78, #4156, #7337, #4891, #8034, #6411, #3271, #173, #8086, #9601, #2433, #5628, #916, #867, #9114, #7430, #323, #8276, #1006, #7483 ),
 .UNSPECIFIED., .F., .T. ) 
 B_SPLINE_CURVE_WITH_KNOTS ( ( 3, 2, 2, 2, 2, 2, 2, 2, 2, 2, 2, 2, 2, 2, 2, 2, 2, 2, 2, 2, 2, 2, 2, 2, 2, 2, 2, 2, 2, 2, 2, 2, 2, 2, 2, 2, 2, 2, 2, 2, 2, 2, 2, 2, 2, 2, 2, 2, 2, 2, 2, 2, 2, 2, 2, 2, 2, 2, 2, 2, 2, 2, 2, 2, 2, 2, 2, 3 ),
 ( 0.000000000000000000, 0.01500076840507158678, 0.03000153681014317356, 0.04500230521521476207, 0.06000307362028634711, 0.07500384202535793909, 0.09000461043042952414, 0.1050053788355011092, 0.1200061472405726942, 0.1350069156456442931, 0.1500076840507158782, 0.1650084524557874632, 0.1800092208608590483, 0.1950099892659306333, 0.2100107576710022184, 0.2250115260760738312, 0.2400122944811453884, 0.2550130628862170012, 0.2700138312912885863, 0.2850145996963601713, 0.3000153681014317564, 0.3150161365065033414, 0.3300169049115749265, 0.3450176733166465115, 0.3600184417217180965, 0.3750192101267896816, 0.3900199785318612666, 0.4050207469369328517, 0.4200215153420044367, 0.4350222837470760773, 0.4500230521521476623, 0.4650238205572192474, 0.4800245889622907769, 0.4950253573673623619, 0.5100261257724340025, 0.5250268941775055875, 0.5400276625825771726, 0.5550284309876486466, 0.5700291993927203427, 0.5850299677977919277, 0.6000307362028635128, 0.6150315046079350978, 0.6300322730130066828, 0.6450330414180782679, 0.6600338098231498529, 0.6750345782282214380, 0.6900353466332930230, 0.7050361150383646081, 0.7200368834434361931, 0.7350376518485077781, 0.7500384202535793632, 0.7650391886586510592, 0.7800399570637225333, 0.7950407254687942293, 0.8100414938738657034, 0.8250422622789372884, 0.8400430306840088734, 0.8550437990890804585, 0.8700445674941521546, 0.8850453358992236286, 0.9000461043042953246, 0.9150468727093667987, 0.9300476411144384947, 0.9450484095195099687, 0.9600491779245815538, 0.9750499463296532499, 0.9900507147347247239, 1.000000000000000000 ),
 .UNSPECIFIED. ) 
 CURVE ( )  GEOMETRIC_REPRESENTATION_ITEM ( )  RATIONAL_B_SPLINE_CURVE ( ( 1.000000000000000000, 0.8660254037844387076, 1.000000000000000000, 0.8660254037844387076, 1.000000000000000000, 0.8660254037844387076, 1.000000000000000000, 0.8660254037844387076, 1.000000000000000000, 0.8660254037844387076, 1.000000000000000000, 0.8660254037844387076, 1.000000000000000000, 0.8660254037844387076, 1.000000000000000000, 0.8660254037844387076, 1.000000000000000000, 0.8660254037844387076, 1.000000000000000000, 0.8660254037844387076, 1.000000000000000000, 0.8660254037844387076, 1.000000000000000000, 0.8660254037844387076, 1.000000000000000000, 0.8660254037844387076, 1.000000000000000000, 0.8660254037844387076, 1.000000000000000000, 0.8660254037844387076, 1.000000000000000000, 0.8660254037844387076, 1.000000000000000000, 0.8660254037844387076, 1.000000000000000000, 0.8660254037844387076, 1.000000000000000000, 0.8660254037844387076, 1.000000000000000000, 0.8660254037844387076, 1.000000000000000000, 0.8660254037844387076, 1.000000000000000000, 0.8660254037844387076, 1.000000000000000000, 0.8660254037844387076, 1.000000000000000000, 0.8660254037844387076, 1.000000000000000000, 0.8660254037844387076, 1.000000000000000000, 0.8660254037844387076, 1.000000000000000000, 0.8660254037844387076, 1.000000000000000000, 0.8660254037844387076, 1.000000000000000000, 0.8660254037844387076, 1.000000000000000000, 0.8660254037844387076, 1.000000000000000000, 0.8660254037844387076, 1.000000000000000000, 0.8660254037844387076, 1.000000000000000000, 0.8660254037844387076, 1.000000000000000000, 0.8660254037844387076, 1.000000000000000000, 0.8660254037844387076, 1.000000000000000000, 0.8660254037844387076, 1.000000000000000000, 0.8660254037844387076, 1.000000000000000000, 0.8660254037844387076, 1.000000000000000000, 0.8660254037844387076, 1.000000000000000000, 0.8660254037844387076, 1.000000000000000000, 0.8660254037844387076, 1.000000000000000000, 0.8660254037844387076, 1.000000000000000000, 0.8660254037844387076, 1.000000000000000000, 0.8660254037844387076, 1.000000000000000000, 0.8660254037844387076, 1.000000000000000000, 0.8660254037844387076, 1.000000000000000000, 0.8660254037844387076, 1.000000000000000000, 0.8660254037844387076, 1.000000000000000000, 0.8660254037844387076, 1.000000000000000000, 0.8660254037844387076, 1.000000000000000000, 0.8660254037844387076, 1.000000000000000000, 0.8660254037844387076, 1.000000000000000000, 0.8660254037844387076, 1.000000000000000000, 0.8660254037844387076, 1.000000000000000000, 0.8660254037844387076, 1.000000000000000000, 0.8660254037844387076, 1.000000000000000000, 0.8660254037844387076, 1.000000000000000000, 0.8660254037844387076, 1.000000000000000000, 0.8660254037844387076, 1.000000000000000000, 0.8660254037844387076, 1.000000000000000000, 0.8660254037844387076, 1.000000000000000000, 0.8660254037844387076, 1.000000000000000000, 0.8660254037844387076, 1.000000000000000000, 0.8660254037844387076, 1.000000000000000000, 0.8660254037844387076, 1.000000000000000000, 0.8660254037844387076, 1.000000000000000000, 0.9111411202376789031, 0.9401538480137057174 ) ) 
 REPRESENTATION_ITEM ( '' )  );
#975 = CARTESIAN_POINT ( 'NONE',  ( -2.256430356249999214, -2.803124999385482763, 1.302750673588581876 ) ) ;
#976 = CIRCLE ( 'NONE', #7648, 27.00000000000000355 ) ;
#977 = ORIENTED_EDGE ( 'NONE', *, *, #8288, .F. ) ;
#978 = LINE ( 'NONE', #1708, #6313 ) ;
#979 = CYLINDRICAL_SURFACE ( 'NONE', #821, 2.500000000000000000 ) ;
#980 = CARTESIAN_POINT ( 'NONE',  ( -27.00000000000001421, 2.649999997815050357, 11.18376618407356560 ) ) ;
#981 = CARTESIAN_POINT ( 'NONE',  ( 4.049441352997683374, 99.50000000000000000, -21.43849541167161732 ) ) ;
#982 = CARTESIAN_POINT ( 'NONE',  ( 3.434779879277784609, 99.99999999999998579, -23.17575050830969374 ) ) ;
#983 = CARTESIAN_POINT ( 'NONE',  ( 4.277141017070624329, 100.0000000000000000, -21.57940364907851816 ) ) ;
#984 = CARTESIAN_POINT ( 'NONE',  ( 3.222930479149370253, 99.49999999999995737, -22.15251218086615381 ) ) ;
#985 = CARTESIAN_POINT ( 'NONE',  ( 27.00000000000000355, 3.049999997815050268, -11.18376618407356737 ) ) ;
#986 = FACE_OUTER_BOUND ( 'NONE', #5345, .T. ) ;
#987 = CARTESIAN_POINT ( 'NONE',  ( 9.877377282685029372E-16, -4.781249998770965348, 2.500000000000000000 ) ) ;
#988 = CARTESIAN_POINT ( 'NONE',  ( 3.552835461024879127, 100.0000000000000000, -21.47801279722421697 ) ) ;
#989 = DIRECTION ( 'NONE',  ( -0.9851965920526258857, 0.000000000000000000, -0.1714283378204774222 ) ) ;
#990 = CARTESIAN_POINT ( 'NONE',  ( 2.500000000000000444, -4.762499999999999289, 1.443375672974063439 ) ) ;
#991 = ORIENTED_EDGE ( 'NONE', *, *, #6106, .F. ) ;
#992 = CARTESIAN_POINT ( 'NONE',  ( -1.128215178124998497, -4.115624999385482319, 1.954126010382872147 ) ) ;
#993 = CARTESIAN_POINT ( 'NONE',  ( 1.034219503716432668E-14, -2.812500000000000444, -2.500000000000000000 ) ) ;
#994 = CARTESIAN_POINT ( 'NONE',  ( 0.000000000000000000, 5.000000000000000000, 0.000000000000000000 ) ) ;
#995 = ADVANCED_FACE ( 'NONE', ( #8137 ), #431, .T. ) ;
#996 = CARTESIAN_POINT ( 'NONE',  ( 19.39806930854667399, 0.9499999989075252893, 19.39806930854668465 ) ) ;
#997 = CARTESIAN_POINT ( 'NONE',  ( 3.105863891863242632, 99.50000000000001421, -22.59672720503480292 ) ) ;
#998 = DIRECTION ( 'NONE',  ( -0.000000000000000000, 1.000000000000000000, -0.000000000000000000 ) ) ;
#999 = CARTESIAN_POINT ( 'NONE',  ( -19.46743691185369585, 99.50000000000000000, -8.912588186774021537 ) ) ;
#1000 = CARTESIAN_POINT ( 'NONE',  ( -21.28703419482447146, 99.49999999999997158, -11.01737971290317297 ) ) ;
#1001 = ORIENTED_EDGE ( 'NONE', *, *, #2037, .T. ) ;
#1002 = CARTESIAN_POINT ( 'NONE',  ( -20.82968571475833031, 99.99999999999994316, -9.677916414284339908 ) ) ;
#1003 = CARTESIAN_POINT ( 'NONE',  ( 3.171774962637509798, 100.0000000000000000, -24.28498992023182268 ) ) ;
#1004 = CARTESIAN_POINT ( 'NONE',  ( 9.576498344683301411, 99.49999999999998579, 20.78592410672095880 ) ) ;
#1005 =( LENGTH_UNIT ( ) NAMED_UNIT ( * ) SI_UNIT ( .MILLI., .METRE. ) );
#1006 = CARTESIAN_POINT ( 'NONE',  ( -2.256430356250000546, -5.226765388979075055, -0.8212675591186288093 ) ) ;
#1007 = CARTESIAN_POINT ( 'NONE',  ( -22.58826642033182353, 99.49999999999998579, -9.883148377786627137 ) ) ;
#1008 = EDGE_CURVE ( 'NONE', #7448, #9173, #9916, .T. ) ;
#1009 = EDGE_CURVE ( 'NONE', #2960, #2104, #4408, .T. ) ;
#1010 = CARTESIAN_POINT ( 'NONE',  ( -16.91659681606879317, 100.0000000000000000, 15.78485274883190392 ) ) ;
#1011 = CARTESIAN_POINT ( 'NONE',  ( 5.226890989224467710, 100.0000000000000000, -23.72545275563321354 ) ) ;
#1012 = CARTESIAN_POINT ( 'NONE',  ( -2.499999999999999556, -3.506249998770965437, 1.443375672974065882 ) ) ;
#1013 = ORIENTED_EDGE ( 'NONE', *, *, #2364, .F. ) ;
#1014 = ORIENTED_EDGE ( 'NONE', *, *, #445, .T. ) ;
#1015 = CARTESIAN_POINT ( 'NONE',  ( -21.29537297865864431, 100.0000000000000000, -11.39144590536739976 ) ) ;
#1016 = CARTESIAN_POINT ( 'NONE',  ( 3.214822648120007731, 99.50000000000000000, -21.86319392453323829 ) ) ;
#1017 = CARTESIAN_POINT ( 'NONE',  ( -14.83363727892122519, 100.0000000000000142, 15.50654517199034466 ) ) ;
#1018 = CARTESIAN_POINT ( 'NONE',  ( 3.486133158594717003E-16, -0.1125000000000000167, -2.500000000000000000 ) ) ;
#1019 = CARTESIAN_POINT ( 'NONE',  ( 8.117007248954752896, 99.50000000000001421, 20.40979824468519155 ) ) ;
#1020 = CARTESIAN_POINT ( 'NONE',  ( 4.100286767325537873, 99.50000000000000000, -22.51382885696750336 ) ) ;
#1021 = CARTESIAN_POINT ( 'NONE',  ( 2.500000000000000000, -3.768749998770965171, -3.061616997868383141E-16 ) ) ;
#1022 =( BOUNDED_CURVE ( )  B_SPLINE_CURVE ( 2, ( #9352, #8512, #10138, #8679, #3751, #559, #3135, #7886, #6937 ),
 .UNSPECIFIED., .F., .F. ) 
 B_SPLINE_CURVE_WITH_KNOTS ( ( 3, 2, 2, 2, 3 ),
 ( 0.7708333333333333703, 0.7777777777777777901, 0.7916666666666666297, 0.8055555555555555802, 0.8125000000000000000 ),
 .UNSPECIFIED. ) 
 CURVE ( )  GEOMETRIC_REPRESENTATION_ITEM ( )  RATIONAL_B_SPLINE_CURVE ( ( 0.9330127018922192983, 0.9330127018922198534, 1.000000000000000000, 0.8660254037844387076, 1.000000000000000000, 0.8660254037844387076, 1.000000000000000000, 0.9330127018922194093, 0.9330127018922194093 ) ) 
 REPRESENTATION_ITEM ( '' )  );
#1023 = ORIENTED_EDGE ( 'NONE', *, *, #7917, .T. ) ;
#1024 = B_SPLINE_CURVE_WITH_KNOTS ( 'NONE', 3,
 ( #10301, #5538, #4014, #1656, #3133, #3079, #8878, #3856, #9513, #4847, #8040, #7043, #2338, #10248, #9462, #4207, #5830, #7301, #9076 ),
 .UNSPECIFIED., .F., .F.,
 ( 4, 1, 1, 1, 1, 1, 1, 1, 1, 1, 1, 1, 1, 1, 1, 1, 4 ),
 ( 0.000000000000000000, 0.07315862907712983310, 0.1430989967074559055, 0.2105333571262071879, 0.2759142635903734653, 0.3397077151413689933, 0.4013946392018796772, 0.4627937533375801049, 0.5237250720276656057, 0.5836284080752294212, 0.6425725562371763511, 0.7010486867616194662, 0.7591976973140022178, 0.8177727706511607186, 0.8769111530050104353, 0.9375229829315941954, 1.000000000000000000 ),
 .UNSPECIFIED. ) ;
#1025 = DIRECTION ( 'NONE',  ( 0.000000000000000000, 0.000000000000000000, -1.000000000000000000 ) ) ;
#1026 = PLANE ( 'NONE',  #6043 ) ;
#1027 = CIRCLE ( 'NONE', #1540, 25.15000000000000213 ) ;
#1028 = EDGE_CURVE ( 'NONE', #6302, #10278, #5133, .T. ) ;
#1029 = CARTESIAN_POINT ( 'NONE',  ( -2.500000000000000000, -4.537499999999999645, -1.443375672974064106 ) ) ;
#1030 = CARTESIAN_POINT ( 'NONE',  ( 3.845216150098881513, 99.99999999999997158, -21.40922359334548020 ) ) ;
#1031 = CARTESIAN_POINT ( 'NONE',  ( 3.291601991079349698, 99.49999999999997158, -22.28586332678438353 ) ) ;
#1032 = CARTESIAN_POINT ( 'NONE',  ( -19.09188309203678813, 2.699999997815051067, 19.09188309203678457 ) ) ;
#1033 = CARTESIAN_POINT ( 'NONE',  ( -20.88772068548257366, 99.50000000000001421, -11.14739719174079546 ) ) ;
#1034 = CARTESIAN_POINT ( 'NONE',  ( -21.38163724633288965, 100.0000000000000568, -9.681902434707239991 ) ) ;
#1035 = DIRECTION ( 'NONE',  ( 0.000000000000000000, 0.000000000000000000, -1.000000000000000000 ) ) ;
#1036 = AXIS2_PLACEMENT_3D ( 'NONE', #6464, #816, #8134 ) ;
#1037 = PLANE ( 'NONE',  #7108 ) ;
#1038 = FACE_OUTER_BOUND ( 'NONE', #2724, .T. ) ;
#1039 = FACE_OUTER_BOUND ( 'NONE', #9827, .T. ) ;
#1040 = EDGE_LOOP ( 'NONE', ( #6213, #6520, #7596, #4974 ) ) ;
#1041 = CARTESIAN_POINT ( 'NONE',  ( -1.128215178124998497, -4.565624999385482496, 1.954126010382872147 ) ) ;
#1042 =( LENGTH_UNIT ( ) NAMED_UNIT ( * ) SI_UNIT ( .MILLI., .METRE. ) );
#1043 = CARTESIAN_POINT ( 'NONE',  ( -14.78677372028383097, 99.99999999999997158, 15.63810349997947569 ) ) ;
#1044 = FACE_OUTER_BOUND ( 'NONE', #3604, .T. ) ;
#1045 = AXIS2_PLACEMENT_3D ( 'NONE', #9396, #9454, #10292 ) ;
#1046 = CARTESIAN_POINT ( 'NONE',  ( -27.43301270000000969, 2.299999998907525267, 11.36312591709335429 ) ) ;
#1047 = DIRECTION ( 'NONE',  ( -0.000000000000000000, -0.000000000000000000, -1.000000000000000000 ) ) ;
#1048 = B_SPLINE_CURVE_WITH_KNOTS ( 'NONE', 3,
 ( #695, #7704, #1429, #3115 ),
 .UNSPECIFIED., .F., .F.,
 ( 4, 4 ),
 ( 0.000000000000000000, 1.000000000000000000 ),
 .UNSPECIFIED. ) ;
#1049 = CARTESIAN_POINT ( 'NONE',  ( -16.35834224700816009, 100.0000000000000142, 16.43761959438736397 ) ) ;
#1050 = CARTESIAN_POINT ( 'NONE',  ( 4.739008722453744049, 100.0000000000000142, -24.06821587619827696 ) ) ;
#1051 = CARTESIAN_POINT ( 'NONE',  ( -20.89145576992255116, 99.99999999999994316, -10.33073932272468198 ) ) ;
#1052 = ORIENTED_EDGE ( 'NONE', *, *, #1402, .F. ) ;
#1053 = CARTESIAN_POINT ( 'NONE',  ( 7.856939908706818798, 99.50000000000001421, 20.19612520319305560 ) ) ;
#1054 = CARTESIAN_POINT ( 'NONE',  ( 27.43301269999999548, 4.999999998907525445, 11.36312591709337916 ) ) ;
#1055 = CARTESIAN_POINT ( 'NONE',  ( 7.486453019397995234, 100.0000000000000000, 23.81666162955709964 ) ) ;
#1056 = FILL_AREA_STYLE_COLOUR ( '', #6062 ) ;
#1057 = CARTESIAN_POINT ( 'NONE',  ( -22.08823018108446234, 99.50000000000000000, -9.406177930363766038 ) ) ;
#1058 = CARTESIAN_POINT ( 'NONE',  ( 9.304660012616079001, 99.50000000000000000, 20.07619068507570859 ) ) ;
#1059 = CARTESIAN_POINT ( 'NONE',  ( 9.513000527211589841, 99.50000000000000000, 20.35102222961602436 ) ) ;
#1060 = CARTESIAN_POINT ( 'NONE',  ( -21.87421819196487505, 100.0000000000000000, -9.684578881761979119 ) ) ;
#1061 = VERTEX_POINT ( 'NONE', #376 ) ;
#1062 = CARTESIAN_POINT ( 'NONE',  ( 2.256430356249999658, -0.4406249993854829961, -1.302750673588581432 ) ) ;
#1063 = ORIENTED_EDGE ( 'NONE', *, *, #7472, .T. ) ;
#1064 = EDGE_CURVE ( 'NONE', #3729, #7819, #7433, .T. ) ;
#1065 = CARTESIAN_POINT ( 'NONE',  ( -22.35673484330673944, 99.99999999999998579, -10.41320610523044721 ) ) ;
#1066 = CARTESIAN_POINT ( 'NONE',  ( 3.611424427577684781, 99.50000000000001421, -21.45475674085064099 ) ) ;
#1067 = LINE ( 'NONE', #1892, #5390 ) ;
#1068 = VECTOR ( 'NONE', #10226, 1000.000000000000000 ) ;
#1069 = FACE_BOUND ( 'NONE', #4305, .T. ) ;
#1070 = CARTESIAN_POINT ( 'NONE',  ( 0.000000000000000000, 73.81339255365637086, 0.000000000000000000 ) ) ;
#1071 = CARTESIAN_POINT ( 'NONE',  ( -22.16320288552370243, 100.0000000000000142, -10.86869938533413915 ) ) ;
#1072 = CARTESIAN_POINT ( 'NONE',  ( 3.296462644833695776, 99.50000000000001421, -23.81854410834942115 ) ) ;
#1073 = VERTEX_POINT ( 'NONE', #5078 ) ;
#1074 = CARTESIAN_POINT ( 'NONE',  ( 4.100286767325537873, 99.50000000000000000, -22.51382885696750336 ) ) ;
#1075 = CARTESIAN_POINT ( 'NONE',  ( -27.43301270000000969, 3.199999998907525178, 11.36312591709335429 ) ) ;
#1076 = CARTESIAN_POINT ( 'NONE',  ( -22.50000000000000355, 72.50000000000001421, 0.000000000000000000 ) ) ;
#1077 = LINE ( 'NONE', #7455, #9617 ) ;
#1078 = CARTESIAN_POINT ( 'NONE',  ( 7.809833820264425519, 99.49999999999995737, 20.29999375863051370 ) ) ;
#1079 = AXIS2_PLACEMENT_3D ( 'NONE', #9249, #3872, #6114 ) ;
#1080 = ORIENTED_EDGE ( 'NONE', *, *, #319, .T. ) ;
#1081 = DIRECTION ( 'NONE',  ( -0.000000000000000000, -1.000000000000000000, -0.000000000000000000 ) ) ;
#1082 = CARTESIAN_POINT ( 'NONE',  ( 11.18376618407357626, 3.649999997815050357, 27.00000000000000000 ) ) ;
#1083 = ADVANCED_FACE ( 'NONE', ( #6026 ), #1268, .F. ) ;
#1084 = CARTESIAN_POINT ( 'NONE',  ( -20.69312081029678296, 99.99999999999997158, -9.926742041671966277 ) ) ;
#1085 = DIRECTION ( 'NONE',  ( 0.000000000000000000, 0.000000000000000000, -1.000000000000000000 ) ) ;
#1086 =( NAMED_UNIT ( * ) SI_UNIT ( $, .STERADIAN. ) SOLID_ANGLE_UNIT ( ) );
#1087 = ADVANCED_FACE ( 'NONE', ( #2045 ), #3629, .T. ) ;
#1088 = CARTESIAN_POINT ( 'NONE',  ( -21.65488089977124275, 99.99999999999997158, -11.10326233039539723 ) ) ;
#1089 = CARTESIAN_POINT ( 'NONE',  ( 3.203979444200292015, 100.0000000000000000, -21.29640115293693725 ) ) ;
#1090 = LINE ( 'NONE', #9045, #7449 ) ;
#1091 = AXIS2_PLACEMENT_3D ( 'NONE', #7906, #2309, #6437 ) ;
#1092 = CARTESIAN_POINT ( 'NONE',  ( 2.500000000000000000, -0.1875000000000000000, -1.443375672974064994 ) ) ;
#1093 = AXIS2_PLACEMENT_3D ( 'NONE', #5684, #7295, #9604 ) ;
#1094 = DIRECTION ( 'NONE',  ( 0.000000000000000000, 0.000000000000000000, -1.000000000000000000 ) ) ;
#1095 = CARTESIAN_POINT ( 'NONE',  ( 27.43301269999999548, 4.199999998907525622, 11.36312591709337738 ) ) ;
#1096 = CARTESIAN_POINT ( 'NONE',  ( -19.09188309203678457, 0.3000000000000000444, -19.09188309203678813 ) ) ;
#1097 = DIRECTION ( 'NONE',  ( -0.000000000000000000, -1.000000000000000000, -0.000000000000000000 ) ) ;
#1098 = CARTESIAN_POINT ( 'NONE',  ( 4.584380863705032283, 100.0000000000000142, -24.21384527865288305 ) ) ;
#1099 =( NAMED_UNIT ( * ) SI_UNIT ( $, .STERADIAN. ) SOLID_ANGLE_UNIT ( ) );
#1100 = ORIENTED_EDGE ( 'NONE', *, *, #2793, .F. ) ;
#1101 = CARTESIAN_POINT ( 'NONE',  ( -20.95972469638759250, 99.50000000000000000, -9.536167108072199028 ) ) ;
#1102 = CARTESIAN_POINT ( 'NONE',  ( -21.16695614262292580, 100.0000000000000000, -11.33496398805607441 ) ) ;
#1103 = CARTESIAN_POINT ( 'NONE',  ( 0.000000000000000000, 0.000000000000000000, 0.000000000000000000 ) ) ;
#1104 =( NAMED_UNIT ( * ) PLANE_ANGLE_UNIT ( ) SI_UNIT ( $, .RADIAN. ) );
#1105 = CARTESIAN_POINT ( 'NONE',  ( 21.79306891025641235, 99.50000000000000000, -1.065004006410256387 ) ) ;
#1106 = CYLINDRICAL_SURFACE ( 'NONE', #885, 27.00000000000000355 ) ;
#1107 = CARTESIAN_POINT ( 'NONE',  ( -16.60513711880302878, 99.50000000000000000, 15.15667007515659570 ) ) ;
#1108 = AXIS2_PLACEMENT_3D ( 'NONE', #6420, #5590, #8776 ) ;
#1109 = CARTESIAN_POINT ( 'NONE',  ( -21.24882413972086681, 100.0000000000000284, -9.742484589929601313 ) ) ;
#1110 = EDGE_LOOP ( 'NONE', ( #9799, #7722, #1954, #9276 ) ) ;
#1111 = CARTESIAN_POINT ( 'NONE',  ( -15.91084591538827198, 100.0000000000000142, 16.65047278764667027 ) ) ;
#1112 = VECTOR ( 'NONE', #3494, 1000.000000000000000 ) ;
#1113 = CARTESIAN_POINT ( 'NONE',  ( -2.500000000000000000, -4.481249998770965526, -1.443375672974064106 ) ) ;
#1114 = VERTEX_POINT ( 'NONE', #1214 ) ;
#1115 = VECTOR ( 'NONE', #5887, 1000.000000000000000 ) ;
#1116 = AXIS2_PLACEMENT_3D ( 'NONE', #4023, #36, #2597 ) ;
#1117 = CARTESIAN_POINT ( 'NONE',  ( -21.84904385032055174, 99.99999999999998579, -11.42736543092427404 ) ) ;
#1118 = CARTESIAN_POINT ( 'NONE',  ( 3.254133136943549776, 99.99999999999997158, -21.76036676155726823 ) ) ;
#1119 = LINE ( 'NONE', #1995, #2870 ) ;
#1120 = CARTESIAN_POINT ( 'NONE',  ( -11.18376618407356737, 3.249999997815050001, -27.00000000000000355 ) ) ;
#1121 = EDGE_CURVE ( 'NONE', #3650, #2978, #9283, .T. ) ;
#1122 = CARTESIAN_POINT ( 'NONE',  ( -2.500000000000000000, -3.637499999999999734, -1.443375672974064106 ) ) ;
#1123 = FACE_OUTER_BOUND ( 'NONE', #3482, .T. ) ;
#1124 = CARTESIAN_POINT ( 'NONE',  ( 9.692323321704657602, 100.0000000000000142, 21.58969587442354410 ) ) ;
#1125 = ORIENTED_EDGE ( 'NONE', *, *, #2957, .F. ) ;
#1126 = DIRECTION ( 'NONE',  ( 0.000000000000000000, -1.000000000000000000, 0.000000000000000000 ) ) ;
#1127 = CARTESIAN_POINT ( 'NONE',  ( -27.43301270000000258, 2.299999998907525267, -11.36312591709336317 ) ) ;
#1128 = CARTESIAN_POINT ( 'NONE',  ( -2.499999999999999112, -4.912499999999999645, 1.443375672974065882 ) ) ;
#1129 = AXIS2_PLACEMENT_3D ( 'NONE', #5815, #8321, #4395 ) ;
#1130 = CARTESIAN_POINT ( 'NONE',  ( 3.350143586568126164, 99.50000000000001421, -24.46212657588250394 ) ) ;
#1131 = CARTESIAN_POINT ( 'NONE',  ( 4.128176300878408256, 99.50000000000001421, -21.47174600747824869 ) ) ;
#1132 = CARTESIAN_POINT ( 'NONE',  ( 3.291601991079349698, 100.0000000000000000, -22.28586332678438353 ) ) ;
#1133 = CARTESIAN_POINT ( 'NONE',  ( -11.18376618407356560, 2.449999997815050179, -27.00000000000000355 ) ) ;
#1134 = DIRECTION ( 'NONE',  ( 0.000000000000000000, 0.000000000000000000, -1.000000000000000000 ) ) ;
#1135 = DIRECTION ( 'NONE',  ( 0.000000000000000000, 0.000000000000000000, -1.000000000000000000 ) ) ;
#1136 = CARTESIAN_POINT ( 'NONE',  ( 3.374624233514611937, 100.0000000000000284, -23.25900349070959550 ) ) ;
#1137 = CARTESIAN_POINT ( 'NONE',  ( -21.86704275050744073, 99.50000000000001421, -11.06111336656620026 ) ) ;
#1138 = CIRCLE ( 'NONE', #6996, 23.99999999999999645 ) ;
#1140 = EDGE_CURVE ( 'NONE', #1713, #7033, #8127, .T. ) ;
#1139 = CARTESIAN_POINT ( 'NONE',  ( 2.837666006185522782, 100.0000000000000000, -22.03040394835428373 ) ) ;
#1141 = CARTESIAN_POINT ( 'NONE',  ( 1.249999999999999334, -4.649999999999999467, -2.165063509461096825 ) ) ;
#1142 = PRODUCT_DEFINITION ( 'UNKNOWN', '', #9806, #6436 ) ;
#1143 = CARTESIAN_POINT ( 'NONE',  ( 2.500000000000000000, -1.087500000000000133, -1.443375672974064994 ) ) ;
#1144 = ADVANCED_FACE ( 'NONE', ( #3679 ), #6862, .T. ) ;
#1145 = CARTESIAN_POINT ( 'NONE',  ( -15.07178375341841559, 99.50000000000001421, 15.16157792772069968 ) ) ;
#1146 = CARTESIAN_POINT ( 'NONE',  ( 3.058419780146050648, 99.50000000000000000, -23.12871267107006545 ) ) ;
#1147 = CARTESIAN_POINT ( 'NONE',  ( 27.43301269999999548, 3.399999998907525356, 11.36312591709337738 ) ) ;
#1148 = ADVANCED_FACE ( 'NONE', ( #5825 ), #1834, .T. ) ;
#1149 = CARTESIAN_POINT ( 'NONE',  ( -27.43301270000000258, 0.7499999989075251117, -3.359575119402369376E-15 ) ) ;
#1150 = DIRECTION ( 'NONE',  ( 0.000000000000000000, 0.000000000000000000, -1.000000000000000000 ) ) ;
#1151 = CARTESIAN_POINT ( 'NONE',  ( 1.034219503716432668E-14, -3.206249998770966059, -2.500000000000000000 ) ) ;
#1152 = CARTESIAN_POINT ( 'NONE',  ( 7.913184448816831029, 100.0000000000000000, 20.09878816755126252 ) ) ;
#1153 = COLOUR_RGB ( '',0.8941176470588234615, 0.8941176470588234615, 0.8941176470588234615 ) ;
#1154 = ORIENTED_EDGE ( 'NONE', *, *, #69, .T. ) ;
#1155 = LINE ( 'NONE', #6800, #9495 ) ;
#1156 = CARTESIAN_POINT ( 'NONE',  ( -2.499999999999999112, -4.012499999999999289, 1.443375672974065882 ) ) ;
#1157 = CARTESIAN_POINT ( 'NONE',  ( 9.877377282685029372E-16, -1.181249998770965703, 2.500000000000000000 ) ) ;
#1158 = CARTESIAN_POINT ( 'NONE',  ( -16.05932294508833280, 99.50000000000000000, 15.21084698918278555 ) ) ;
#1159 = CARTESIAN_POINT ( 'NONE',  ( -0.6698729810778043525, -1.836153809338631593, -2.500000000000001332 ) ) ;
#1160 = EDGE_CURVE ( 'NONE', #3123, #405, #8323, .T. ) ;
#1161 = CARTESIAN_POINT ( 'NONE',  ( 9.526533506306627430, 99.99999999999994316, 21.03094362668609207 ) ) ;
#1162 = DIRECTION ( 'NONE',  ( 0.000000000000000000, -1.000000000000000000, 0.000000000000000000 ) ) ;
#1163 = VERTEX_POINT ( 'NONE', #2953 ) ;
#1164 = FACE_OUTER_BOUND ( 'NONE', #1230, .T. ) ;
#1165 = CARTESIAN_POINT ( 'NONE',  ( -2.256430356250000102, -0.7031249993854828961, 0.000000000000000000 ) ) ;
#1166 = ORIENTED_EDGE ( 'NONE', *, *, #5394, .T. ) ;
#1167 = CARTESIAN_POINT ( 'NONE',  ( -21.94169572595625795, 99.50000000000000000, -9.715372641902229489 ) ) ;
#1168 = CARTESIAN_POINT ( 'NONE',  ( 24.93339342948717885, 99.50000000000000000, -1.235376602564102644 ) ) ;
#1169 = CARTESIAN_POINT ( 'NONE',  ( 3.573144549190039321, 99.49999999999998579, -23.04580706645134214 ) ) ;
#1170 = CARTESIAN_POINT ( 'NONE',  ( -3.486133158594716510E-16, -3.712499999999999467, -2.500000000000000000 ) ) ;
#1171 = CARTESIAN_POINT ( 'NONE',  ( -11.18376618407356737, 2.649999999999999467, -27.00000000000000355 ) ) ;
#1172 =( BOUNDED_CURVE ( )  B_SPLINE_CURVE ( 2, ( #6152, #3643, #3808, #5319, #2061, #4525, #8508, #6039, #9349 ),
 .UNSPECIFIED., .F., .F. ) 
 B_SPLINE_CURVE_WITH_KNOTS ( ( 3, 2, 2, 2, 3 ),
 ( 0.5208333333333333703, 0.5277777777777777901, 0.5416666666666666297, 0.5555555555555555802, 0.5625000000000000000 ),
 .UNSPECIFIED. ) 
 CURVE ( )  GEOMETRIC_REPRESENTATION_ITEM ( )  RATIONAL_B_SPLINE_CURVE ( ( 0.9330127018922192983, 0.9330127018922198534, 1.000000000000000000, 0.8660254037844387076, 1.000000000000000000, 0.8660254037844387076, 1.000000000000000000, 0.9330127018922194093, 0.9330127018922194093 ) ) 
 REPRESENTATION_ITEM ( '' )  );
#1173 = DIRECTION ( 'NONE',  ( -0.000000000000000000, 1.000000000000000000, -0.000000000000000000 ) ) ;
#1174 = ORIENTED_EDGE ( 'NONE', *, *, #1949, .F. ) ;
#1175 = CARTESIAN_POINT ( 'NONE',  ( -22.11394672483139701, 100.0000000000000000, -10.91855052283267646 ) ) ;
#1176 = CARTESIAN_POINT ( 'NONE',  ( 9.547662139763570366, 99.99999999999997158, 20.94662037603165672 ) ) ;
#1177 = EDGE_LOOP ( 'NONE', ( #10034, #3325, #6787, #6308, #2950, #2735 ) ) ;
#1178 = B_SPLINE_CURVE_WITH_KNOTS ( 'NONE', 3,
 ( #825, #3417, #973, #8145, #4164, #4901, #7348, #9611, #4118, #7250, #4794, #1747, #6611, #233, #5738, #8189, #7993, #1603, #8927 ),
 .UNSPECIFIED., .F., .F.,
 ( 4, 1, 1, 1, 1, 1, 1, 1, 1, 1, 1, 1, 1, 1, 1, 1, 4 ),
 ( 0.000000000000000000, 0.06463354665699841406, 0.1274839167070160040, 0.1893660780973640267, 0.2502738481868047038, 0.3108090901939400408, 0.3728692346228669741, 0.4358265942208103261, 0.5002515515682643965, 0.5647461136436963125, 0.6273730017603231790, 0.6892793264321037672, 0.7497280364991398827, 0.8111249352628771003, 0.8723480300361200479, 0.9354359082354426480, 1.000000000000000000 ),
 .UNSPECIFIED. ) ;
#1179 = DIRECTION ( 'NONE',  ( 0.7071067811865473507, 0.000000000000000000, 0.7071067811865477948 ) ) ;
#1180 = CARTESIAN_POINT ( 'NONE',  ( 27.43301270000000258, 5.149999998907525800, 0.000000000000000000 ) ) ;
#1181 = CARTESIAN_POINT ( 'NONE',  ( 9.877377282685029372E-16, -2.081249998770965615, 2.500000000000000000 ) ) ;
#1182 = CARTESIAN_POINT ( 'NONE',  ( 9.915951879163557692, 99.50000000000002842, 20.63215000232408158 ) ) ;
#1183 = CARTESIAN_POINT ( 'NONE',  ( 26.99999999999999645, 4.549999997815051600, 11.18376618407358691 ) ) ;
#1184 = VERTEX_POINT ( 'NONE', #9270 ) ;
#1185 = CARTESIAN_POINT ( 'NONE',  ( 3.252389375388976323, 99.50000000000004263, -22.22144413113850447 ) ) ;
#1186 = CARTESIAN_POINT ( 'NONE',  ( 19.09188309203678813, 3.099999997815050090, -19.09188309203678813 ) ) ;
#1187 = LINE ( 'NONE', #2071, #2352 ) ;
#1188 = CYLINDRICAL_SURFACE ( 'NONE', #645, 27.00000000000000000 ) ;
#1189 = CARTESIAN_POINT ( 'NONE',  ( 3.973150561375555334, 100.0000000000000000, -22.87236500961342855 ) ) ;
#1190 = ORIENTED_EDGE ( 'NONE', *, *, #2658, .F. ) ;
#1191 = CARTESIAN_POINT ( 'NONE',  ( -4.959819536546781389E-15, 2.799999997815050268, 27.00000000000000355 ) ) ;
#1192 = CARTESIAN_POINT ( 'NONE',  ( -2.500000000000000000, -0.03749999999999999167, -1.443375672974064106 ) ) ;
#1193 = ORIENTED_EDGE ( 'NONE', *, *, #9, .T. ) ;
#1194 = EDGE_CURVE ( 'NONE', #84, #4497, #259, .T. ) ;
#1195 = CARTESIAN_POINT ( 'NONE',  ( 1.249999999999999334, -1.499999999999999778, -2.165063509461096825 ) ) ;
#1196 = APPLICATION_PROTOCOL_DEFINITION ( 'draft international standard', 'automotive_design', 1998, #6724 ) ;
#1197 = CARTESIAN_POINT ( 'NONE',  ( -14.89508182811745662, 99.99999999999995737, 15.38112983991209326 ) ) ;
#1198 = CARTESIAN_POINT ( 'NONE',  ( 9.820792995160308791, 100.0000000000000000, 20.21220011423140761 ) ) ;
#1199 = CARTESIAN_POINT ( 'NONE',  ( -11.36312591709337383, 3.999999998907525889, 27.43301269999999548 ) ) ;
#1200 = ORIENTED_EDGE ( 'NONE', *, *, #2801, .T. ) ;
#1201 = VECTOR ( 'NONE', #8870, 1000.000000000000000 ) ;
#1202 = CARTESIAN_POINT ( 'NONE',  ( -15.98323291606820362, 99.99999999999998579, 16.64087298452848884 ) ) ;
#1203 = CARTESIAN_POINT ( 'NONE',  ( 21.47055288461538325, 100.0000000000000000, -0.7081330128205128860 ) ) ;
#1204 = CARTESIAN_POINT ( 'NONE',  ( 3.478562133589548910, 99.99999999999997158, -24.13114810667639532 ) ) ;
#1205 = CARTESIAN_POINT ( 'NONE',  ( 8.322475189980043098, 99.50000000000001421, 19.72675386960232657 ) ) ;
#1206 = CARTESIAN_POINT ( 'NONE',  ( -1.249999999999998224, -3.974999999999999201, 2.165063509461097713 ) ) ;
#1207 = ORIENTED_EDGE ( 'NONE', *, *, #500, .T. ) ;
#1208 = CARTESIAN_POINT ( 'NONE',  ( -2.499999999999999112, -1.256249998770965659, 1.443375672974065882 ) ) ;
#1209 = CARTESIAN_POINT ( 'NONE',  ( -27.43301270000000258, 0.6499999989075252449, -3.359575119402369376E-15 ) ) ;
#1210 = CIRCLE ( 'NONE', #9577, 25.00000000000000000 ) ;
#1211 = SHAPE_REPRESENTATION_RELATIONSHIP ( 'NONE' , 'NONE' ,  #5481, #6379 ) ;
#1212 = CARTESIAN_POINT ( 'NONE',  ( 4.363164797760430424, 100.0000000000000284, -21.67376679147534446 ) ) ;
#1213 = DIRECTION ( 'NONE',  ( 0.000000000000000000, 1.000000000000000000, 0.000000000000000000 ) ) ;
#1214 = CARTESIAN_POINT ( 'NONE',  ( -16.36254897777739004, 100.0000000000000142, 15.39785597259249350 ) ) ;
#1215 = ORIENTED_EDGE ( 'NONE', *, *, #3912, .F. ) ;
#1216 = CARTESIAN_POINT ( 'NONE',  ( -16.05266356869597644, 100.0000000000000000, 16.62382211633880047 ) ) ;
#1217 = AXIS2_PLACEMENT_3D ( 'NONE', #5160, #5801, #5005 ) ;
#1218 = EDGE_CURVE ( 'NONE', #1184, #6802, #8495, .T. ) ;
#1219 = CARTESIAN_POINT ( 'NONE',  ( 1.128215178125001161, -1.003124999385482718, 1.954126010382870815 ) ) ;
#1220 = ORIENTED_EDGE ( 'NONE', *, *, #7472, .F. ) ;
#1221 = ADVANCED_FACE ( 'NONE', ( #752 ), #1677, .T. ) ;
#1222 = CARTESIAN_POINT ( 'NONE',  ( 4.640952353770416927, 99.50000000000000000, -24.17064508475253604 ) ) ;
#1223 = LINE ( 'NONE', #6032, #5287 ) ;
#1224 = CARTESIAN_POINT ( 'NONE',  ( 3.293841816516395848, 99.49999999999998579, -23.44781013845121009 ) ) ;
#1225 = CARTESIAN_POINT ( 'NONE',  ( -11.18376618407358336, 3.549999997815050268, 26.99999999999999645 ) ) ;
#1226 = ORIENTED_EDGE ( 'NONE', *, *, #4224, .F. ) ;
#1227 = LINE ( 'NONE', #8451, #473 ) ;
#1228 = DIRECTION ( 'NONE',  ( 0.000000000000000000, -1.000000000000000000, 0.000000000000000000 ) ) ;
#1229 = CARTESIAN_POINT ( 'NONE',  ( -15.09818093130665773, 100.0000000000000000, 16.69478731934044191 ) ) ;
#1230 = EDGE_LOOP ( 'NONE', ( #5144, #5256, #1827, #169, #4560, #2743 ) ) ;
#1231 = CARTESIAN_POINT ( 'NONE',  ( 0.000000000000000000, 0.000000000000000000, 0.000000000000000000 ) ) ;
#1232 = CARTESIAN_POINT ( 'NONE',  ( -11.36312591709337383, 3.299999998907525267, 27.43301269999999548 ) ) ;
#1233 = CARTESIAN_POINT ( 'NONE',  ( -2.500000000000000000, -2.193749998770965881, 0.000000000000000000 ) ) ;
#1234 = CARTESIAN_POINT ( 'NONE',  ( -16.88522588321459494, 99.50000000000002842, 16.18266969485829421 ) ) ;
#1235 = ORIENTED_EDGE ( 'NONE', *, *, #9720, .F. ) ;
#1236 = CARTESIAN_POINT ( 'NONE',  ( 1.679787559701184688E-15, 5.349999998907525089, -27.43301270000000258 ) ) ;
#1237 = CARTESIAN_POINT ( 'NONE',  ( 8.536201443755420115, 99.50000000000002842, 19.63502355897212581 ) ) ;
#1238 =( BOUNDED_CURVE ( )  B_SPLINE_CURVE ( 2, ( #3288, #3974, #9669, #7206, #38, #9620, #8837, #4858, #8688 ),
 .UNSPECIFIED., .F., .F. ) 
 B_SPLINE_CURVE_WITH_KNOTS ( ( 3, 2, 2, 2, 3 ),
 ( 0.3928571428571428492, 0.4107142857142856984, 0.4285714285714285476, 0.4464285714285714524, 0.4642857142857143016 ),
 .UNSPECIFIED. ) 
 CURVE ( )  GEOMETRIC_REPRESENTATION_ITEM ( )  RATIONAL_B_SPLINE_CURVE ( ( 1.000000000000000000, 0.9238795325112867385, 1.000000000000000000, 0.9238795325112867385, 1.000000000000000000, 0.9238795325112867385, 1.000000000000000000, 0.9238795325112867385, 1.000000000000000000 ) ) 
 REPRESENTATION_ITEM ( '' )  );
#1239 = CARTESIAN_POINT ( 'NONE',  ( -3.486133158594716510E-16, -4.106249998770965526, -2.500000000000000000 ) ) ;
#1240 = CYLINDRICAL_SURFACE ( 'NONE', #5814, 2.500000000000000000 ) ;
#1241 = CARTESIAN_POINT ( 'NONE',  ( 3.275092494823534928, 100.0000000000000000, -23.54688978826290580 ) ) ;
#1242 = VERTEX_POINT ( 'NONE', #8712 ) ;
#1243 = DIRECTION ( 'NONE',  ( 0.000000000000000000, 1.000000000000000000, 0.000000000000000000 ) ) ;
#1244 = VECTOR ( 'NONE', #1372, 1000.000000000000000 ) ;
#1245 = CARTESIAN_POINT ( 'NONE',  ( 27.43301270000000258, 2.749999998907525445, 0.000000000000000000 ) ) ;
#1246 = ORIENTED_EDGE ( 'NONE', *, *, #8836, .T. ) ;
#1247 = CARTESIAN_POINT ( 'NONE',  ( 1.250000000000001110, -0.7499999999999998890, 2.165063509461096380 ) ) ;
#1248 = PRODUCT_CONTEXT ( 'NONE', #5122, 'mechanical' ) ;
#1249 = CARTESIAN_POINT ( 'NONE',  ( 3.311778287470797721, 99.99999999999997158, -21.22295334266859967 ) ) ;
#1250 = CARTESIAN_POINT ( 'NONE',  ( -1.128215178124998497, -1.528124999385482852, 1.954126010382872147 ) ) ;
#1251 = CARTESIAN_POINT ( 'NONE',  ( 19.39806930854667399, 4.149999998907525800, 19.39806930854668465 ) ) ;
#1252 = CARTESIAN_POINT ( 'NONE',  ( -11.36312591709337383, 3.299999998907525267, 27.43301269999999548 ) ) ;
#1253 = EDGE_CURVE ( 'NONE', #2978, #3650, #940, .T. ) ;
#1254 = CARTESIAN_POINT ( 'NONE',  ( 9.820792995160308791, 100.0000000000000000, 20.21220011423140761 ) ) ;
#1255 = DIRECTION ( 'NONE',  ( -0.8799640205556051864, 0.000000000000000000, -0.4750403377899757862 ) ) ;
#1256 = CARTESIAN_POINT ( 'NONE',  ( 0.000000000000000000, 87.00000000000001421, 0.000000000000000000 ) ) ;
#1257 = VECTOR ( 'NONE', #10093, 1000.000000000000000 ) ;
#1258 = CARTESIAN_POINT ( 'NONE',  ( 3.428794695218988053, 100.0000000000000142, -24.07607503615978572 ) ) ;
#1259 = ADVANCED_BREP_SHAPE_REPRESENTATION ( '', ( #6543, #5055 ), #8584 ) ;
#1260 = VERTEX_POINT ( 'NONE', #3892 ) ;
#1261 = CARTESIAN_POINT ( 'NONE',  ( -1.128215178125000273, -2.015624999385483118, -1.954126010382871259 ) ) ;
#1262 = CARTESIAN_POINT ( 'NONE',  ( 0.000000000000000000, 97.00000000000000000, 0.000000000000000000 ) ) ;
#1263 = EDGE_LOOP ( 'NONE', ( #5643, #8438, #8442, #4121 ) ) ;
#1264 = CARTESIAN_POINT ( 'NONE',  ( -1.128215178124998497, -0.9656249993854827407, 1.954126010382872147 ) ) ;
#1265 = CARTESIAN_POINT ( 'NONE',  ( -5.039362679103552881E-15, 0.8499999989075252005, 27.43301270000000258 ) ) ;
#1266 = CARTESIAN_POINT ( 'NONE',  ( -15.84712739808237103, 99.99999999999994316, 14.83079670662049310 ) ) ;
#1267 = CARTESIAN_POINT ( 'NONE',  ( 9.500395184910136237, 99.99999999999994316, 21.12540332933289733 ) ) ;
#1268 = CYLINDRICAL_SURFACE ( 'NONE', #3424, 25.00000000000000000 ) ;
#1269 = ORIENTED_EDGE ( 'NONE', *, *, #4456, .T. ) ;
#1270 = CYLINDRICAL_SURFACE ( 'NONE', #2390, 27.00000000000000355 ) ;
#1271 = CARTESIAN_POINT ( 'NONE',  ( -2.256430356250000102, -2.990624999385482763, -1.302750673588580321 ) ) ;
#1272 = EDGE_LOOP ( 'NONE', ( #9387, #10151 ) ) ;
#1273 = CARTESIAN_POINT ( 'NONE',  ( -22.06741020400400188, 100.0000000000000142, -9.788922322134999021 ) ) ;
#1274 = CARTESIAN_POINT ( 'NONE',  ( 1.249999999999999334, -0.5999999999999999778, -2.165063509461096825 ) ) ;
#1275 = CARTESIAN_POINT ( 'NONE',  ( 3.486133158594717003E-16, -0.1125000000000000167, -2.500000000000000000 ) ) ;
#1276 = VECTOR ( 'NONE', #1944, 1000.000000000000000 ) ;
#1277 = DIRECTION ( 'NONE',  ( 0.000000000000000000, 1.000000000000000000, 0.000000000000000000 ) ) ;
#1278 = CARTESIAN_POINT ( 'NONE',  ( 3.207968951880266761, 99.99999999999998579, -22.92616835434091627 ) ) ;
#1279 = ADVANCED_FACE ( 'NONE', ( #3789 ), #4725, .T. ) ;
#1280 = VECTOR ( 'NONE', #8827, 1000.000000000000114 ) ;
#1281 = CARTESIAN_POINT ( 'NONE',  ( 3.712044765110731337, 99.49999999999998579, -21.08683700305641651 ) ) ;
#1282 = CARTESIAN_POINT ( 'NONE',  ( -19.09188309203678457, 1.100000000000000089, -19.09188309203678813 ) ) ;
#1283 = DIRECTION ( 'NONE',  ( -0.9804671828129908340, 0.000000000000000000, 0.1966827481675937905 ) ) ;
#1284 = ORIENTED_EDGE ( 'NONE', *, *, #911, .F. ) ;
#1285 = CARTESIAN_POINT ( 'NONE',  ( 2.562556682370379146, -20.00000000000000000, 1.479492790380214418 ) ) ;
#1286 = CARTESIAN_POINT ( 'NONE',  ( -11.36312591709337383, 2.499999998907525445, 27.43301269999999548 ) ) ;
#1287 = CARTESIAN_POINT ( 'NONE',  ( 2.256430356250000546, -2.203124999385482674, 1.302750673588579877 ) ) ;
#1288 = DIRECTION ( 'NONE',  ( 0.05376826219280737146, 0.000000000000000000, 0.9985534407235125975 ) ) ;
#1289 = ORIENTED_EDGE ( 'NONE', *, *, #9640, .T. ) ;
#1290 = CARTESIAN_POINT ( 'NONE',  ( -20.89052720883767122, 100.0000000000000000, -9.602653601535816819 ) ) ;
#1291 = CARTESIAN_POINT ( 'NONE',  ( 5.240996349771887886, 99.50000000000001421, -23.60769396873743631 ) ) ;
#1292 = CARTESIAN_POINT ( 'NONE',  ( 0.000000000000000000, 105.0000000000000142, 0.000000000000000000 ) ) ;
#1293 = CARTESIAN_POINT ( 'NONE',  ( -16.54770463920453949, 99.50000000000002842, 15.70234036036222847 ) ) ;
#1294 = ORIENTED_EDGE ( 'NONE', *, *, #8620, .F. ) ;
#1295 = CARTESIAN_POINT ( 'NONE',  ( -16.63177974700816009, 100.0000000000000000, 16.59747536361813403 ) ) ;
#1296 = CARTESIAN_POINT ( 'NONE',  ( 1.679787559701184688E-15, 2.949999998907525178, -27.43301270000000258 ) ) ;
#1297 = ORIENTED_EDGE ( 'NONE', *, *, #1332, .F. ) ;
#1298 = TOROIDAL_SURFACE ( 'NONE', #7156, 23.82500000000000284, 1.324999999999999956 ) ;
#1299 = CARTESIAN_POINT ( 'NONE',  ( -2.500000000000000000, -1.800000000000000044, 0.000000000000000000 ) ) ;
#1300 = APPLICATION_PROTOCOL_DEFINITION ( 'draft international standard', 'automotive_design', 1998, #5679 ) ;
#1301 = CARTESIAN_POINT ( 'NONE',  ( 0.000000000000000000, 100.0000000000000000, 0.000000000000000000 ) ) ;
#1302 = CARTESIAN_POINT ( 'NONE',  ( 0.000000000000000000, 100.0000000000000000, 0.000000000000000000 ) ) ;
#1303 =( BOUNDED_CURVE ( )  B_SPLINE_CURVE ( 2, ( #5578, #3220, #8766, #7238, #4783, #7928, #760, #8866, #4054 ),
 .UNSPECIFIED., .F., .T. ) 
 B_SPLINE_CURVE_WITH_KNOTS ( ( 3, 2, 2, 2, 3 ),
 ( 0.3214285714285714524, 0.3392857142857143016, 0.3571428571428571508, 0.3750000000000000000, 0.3928571428571428492 ),
 .UNSPECIFIED. ) 
 CURVE ( )  GEOMETRIC_REPRESENTATION_ITEM ( )  RATIONAL_B_SPLINE_CURVE ( ( 1.000000000000000000, 0.9238795325112867385, 1.000000000000000000, 0.9238795325112867385, 1.000000000000000000, 0.9238795325112867385, 1.000000000000000000, 0.9238795325112867385, 1.000000000000000000 ) ) 
 REPRESENTATION_ITEM ( '' )  );
#1304 = CARTESIAN_POINT ( 'NONE',  ( -2.256430356250000102, -2.503124999385482496, 0.000000000000000000 ) ) ;
#1305 = CARTESIAN_POINT ( 'NONE',  ( -16.90689012439429462, 99.49999999999998579, 16.08742389234230785 ) ) ;
#1306 = CARTESIAN_POINT ( 'NONE',  ( -27.43301270000000258, 1.499999998907525223, -11.36312591709336317 ) ) ;
#1307 = ORIENTED_EDGE ( 'NONE', *, *, #6517, .T. ) ;
#1308 = UNCERTAINTY_MEASURE_WITH_UNIT (LENGTH_MEASURE( 1.000000000000000082E-05 ), #6022, 'distance_accuracy_value', 'NONE');
#1309 = CARTESIAN_POINT ( 'NONE',  ( -15.84712739808237103, 99.99999999999997158, 14.83079670662049310 ) ) ;
#1310 = FACE_OUTER_BOUND ( 'NONE', #8227, .T. ) ;
#1311 = CARTESIAN_POINT ( 'NONE',  ( 0.000000000000000000, 105.0000000000000142, 0.000000000000000000 ) ) ;
#1312 = CARTESIAN_POINT ( 'NONE',  ( -16.25072943800822500, 100.0000000000000568, 15.30228603765648820 ) ) ;
#1313 = VERTEX_POINT ( 'NONE', #3944 ) ;
#1314 = CARTESIAN_POINT ( 'NONE',  ( 4.786228327491940187E-16, -0.9281249993854828739, 2.605501347177161087 ) ) ;
#1315 = CARTESIAN_POINT ( 'NONE',  ( 2.859712287474666770, 100.0000000000000000, -22.17872625191749236 ) ) ;
#1316 = ORIENTED_EDGE ( 'NONE', *, *, #8630, .F. ) ;
#1317 = CARTESIAN_POINT ( 'NONE',  ( -2.500000000000000000, -1.331249998770965837, -1.443375672974064106 ) ) ;
#1318 = CARTESIAN_POINT ( 'NONE',  ( -27.43301270000000969, 3.099999998907525089, 11.36312591709335429 ) ) ;
#1319 = ADVANCED_FACE ( 'NONE', ( #10059 ), #6360, .T. ) ;
#1320 = CARTESIAN_POINT ( 'NONE',  ( -15.98658610793439117, 99.50000000000001421, 14.83943845084690949 ) ) ;
#1321 = B_SPLINE_CURVE_WITH_KNOTS ( 'NONE', 3,
 ( #4880, #9642, #2476, #5672, #8076, #905, #3311, #7372, #4339, #8370, #7473 ),
 .UNSPECIFIED., .F., .F.,
 ( 4, 1, 1, 1, 1, 1, 1, 1, 4 ),
 ( 0.000000000000000000, 0.09767211715481777246, 0.1989896052561311024, 0.3043518128873296535, 0.4150874769980872347, 0.5363819683935961979, 0.6738601886791220075, 0.8283091006677448798, 1.000000000000000000 ),
 .UNSPECIFIED. ) ;
#1322 = CARTESIAN_POINT ( 'NONE',  ( -19.09188309203678457, 1.899999999999999911, -19.09188309203678813 ) ) ;
#1323 = CARTESIAN_POINT ( 'NONE',  ( 8.973011566395204142, 99.49999999999997158, 19.93291184930431115 ) ) ;
#1324 = EDGE_LOOP ( 'NONE', ( #4697, #1014 ) ) ;
#1325 = PLANE ( 'NONE',  #40 ) ;
#1326 = CARTESIAN_POINT ( 'NONE',  ( 1.128215178125001161, -1.453124999385482896, 1.954126010382870815 ) ) ;
#1327 = ORIENTED_EDGE ( 'NONE', *, *, #521, .T. ) ;
#1328 = B_SPLINE_CURVE_WITH_KNOTS ( 'NONE', 3,
 ( #1049, #3722, #7800, #5346, #10044, #7580, #7750, #1202, #630, #4445, #4394, #8535, #3614, #6230, #3773, #3669, #8479, #417, #6960 ),
 .UNSPECIFIED., .F., .F.,
 ( 4, 1, 1, 1, 1, 1, 1, 1, 1, 1, 1, 1, 1, 1, 1, 1, 4 ),
 ( 0.000000000000000000, 0.06473117683888822416, 0.1283191082976379849, 0.1900130092022370987, 0.2509653124206144836, 0.3118694605430146760, 0.3735603890354366463, 0.4359106579620777855, 0.5007804971236301528, 0.5656503362851855732, 0.6280858374182423098, 0.6899222460797727052, 0.7510277903999277305, 0.8114330998898260372, 0.8726106248506092511, 0.9357151229638154266, 1.000000000000000000 ),
 .UNSPECIFIED. ) ;
#1329 = CYLINDRICAL_SURFACE ( 'NONE', #2785, 25.00000000000000000 ) ;
#1330 = CARTESIAN_POINT ( 'NONE',  ( -15.89341924297059094, 100.0000000000000142, 17.07725933521297890 ) ) ;
#1331 = DIRECTION ( 'NONE',  ( -0.1697592580069431922, 0.000000000000000000, 0.9854855627156250408 ) ) ;
#1332 = EDGE_CURVE ( 'NONE', #9169, #7011, #4267, .T. ) ;
#1333 = PRODUCT ( 'time set dial', 'time set dial', '', ( #2137 ) ) ;
#1334 = CARTESIAN_POINT ( 'NONE',  ( 2.256430356249999658, -1.790624999385483029, -1.302750673588581432 ) ) ;
#1335 = CARTESIAN_POINT ( 'NONE',  ( -11.18376618407356737, 3.450000000000000178, -27.00000000000000355 ) ) ;
#1336 = CARTESIAN_POINT ( 'NONE',  ( 3.771794781161601939, 99.49999999999998579, -21.07813736596861176 ) ) ;
#1337 = CARTESIAN_POINT ( 'NONE',  ( -0.6698729810778069060, -2.736153809338631504, -2.500000000000000000 ) ) ;
#1338 = CARTESIAN_POINT ( 'NONE',  ( 19.09188309203678813, 0.9000000000000001332, -19.09188309203678813 ) ) ;
#1339 = EDGE_LOOP ( 'NONE', ( #9519, #2190, #10075, #2428 ) ) ;
#1340 = CARTESIAN_POINT ( 'NONE',  ( -21.56977948371741505, 99.49999999999995737, -11.44450812306045329 ) ) ;
#1341 = CYLINDRICAL_SURFACE ( 'NONE', #5874, 2.500000000000000000 ) ;
#1342 = CARTESIAN_POINT ( 'NONE',  ( 1.128215178124999607, -1.640624999385482896, -1.954126010382871259 ) ) ;
#1343 = CARTESIAN_POINT ( 'NONE',  ( 9.881472129446523311, 99.50000000000002842, 20.94326683228310060 ) ) ;
#1344 = CARTESIAN_POINT ( 'NONE',  ( 1.045839947578414805E-15, -0.9562499987709659477, -2.500000000000000000 ) ) ;
#1345 = LINE ( 'NONE', #511, #8390 ) ;
#1346 = FILL_AREA_STYLE_COLOUR ( '', #3513 ) ;
#1347 = FACE_BOUND ( 'NONE', #8726, .T. ) ;
#1348 = ORIENTED_EDGE ( 'NONE', *, *, #8427, .T. ) ;
#1349 = CARTESIAN_POINT ( 'NONE',  ( 0.000000000000000000, 97.50000000000000000, 0.000000000000000000 ) ) ;
#1350 = CARTESIAN_POINT ( 'NONE',  ( -19.39806930854667755, 3.049999998907525711, -19.39806930854668110 ) ) ;
#1351 = ORIENTED_EDGE ( 'NONE', *, *, #4166, .F. ) ;
#1352 = EDGE_CURVE ( 'NONE', #1061, #570, #8955, .T. ) ;
#1353 = CARTESIAN_POINT ( 'NONE',  ( -2.500000000000000000, -1.837499999999999911, -1.443375672974064106 ) ) ;
#1354 = CARTESIAN_POINT ( 'NONE',  ( 27.00000000000000355, 0.000000000000000000, 0.000000000000000000 ) ) ;
#1355 = FACE_OUTER_BOUND ( 'NONE', #8614, .T. ) ;
#1356 = CARTESIAN_POINT ( 'NONE',  ( -2.256430356250000102, -2.090624999385482852, -1.302750673588580321 ) ) ;
#1357 = CARTESIAN_POINT ( 'NONE',  ( -16.60513711880302878, 99.50000000000000000, 15.15667007515659570 ) ) ;
#1358 = CARTESIAN_POINT ( 'NONE',  ( -27.43301270000000258, 3.149999998907524912, -3.359575119402369376E-15 ) ) ;
#1359 = ORIENTED_EDGE ( 'NONE', *, *, #8169, .F. ) ;
#1360 = CARTESIAN_POINT ( 'NONE',  ( 9.445361748092775400, 100.0000000000000142, 19.75398588445988324 ) ) ;
#1361 = CARTESIAN_POINT ( 'NONE',  ( 2.939152317953648289E-15, 97.00000000000000000, 24.00000000000000355 ) ) ;
#1362 = CARTESIAN_POINT ( 'NONE',  ( 7.486453019397995234, 100.0000000000000000, 23.81666162955709964 ) ) ;
#1363 = FACE_OUTER_BOUND ( 'NONE', #5779, .T. ) ;
#1364 = CARTESIAN_POINT ( 'NONE',  ( -2.256430356250000102, -0.5906249993854829627, 0.000000000000000000 ) ) ;
#1365 = CARTESIAN_POINT ( 'NONE',  ( -2.499999999999999556, -5.367390331571028739, -0.9099168337232446113 ) ) ;
#1366 = VERTEX_POINT ( 'NONE', #4775 ) ;
#1367 = PLANE ( 'NONE',  #7746 ) ;
#1368 =( BOUNDED_CURVE ( )  B_SPLINE_CURVE ( 2, ( #856, #4047, #7230, #7129, #3262, #6352, #7330, #3353, #10334 ),
 .UNSPECIFIED., .F., .F. ) 
 B_SPLINE_CURVE_WITH_KNOTS ( ( 3, 2, 2, 2, 3 ),
 ( 0.5208333333333333703, 0.5277777777777777901, 0.5416666666666666297, 0.5555555555555555802, 0.5625000000000000000 ),
 .UNSPECIFIED. ) 
 CURVE ( )  GEOMETRIC_REPRESENTATION_ITEM ( )  RATIONAL_B_SPLINE_CURVE ( ( 0.9330127018922192983, 0.9330127018922198534, 1.000000000000000000, 0.8660254037844387076, 1.000000000000000000, 0.8660254037844387076, 1.000000000000000000, 0.9330127018922194093, 0.9330127018922194093 ) ) 
 REPRESENTATION_ITEM ( '' )  );
#1369 = CARTESIAN_POINT ( 'NONE',  ( -27.43301270000000258, 3.849999998907525534, -3.359575119402369376E-15 ) ) ;
#1370 =( NAMED_UNIT ( * ) PLANE_ANGLE_UNIT ( ) SI_UNIT ( $, .RADIAN. ) );
#1371 = VERTEX_POINT ( 'NONE', #6400 ) ;
#1372 = DIRECTION ( 'NONE',  ( -0.000000000000000000, -1.000000000000000000, -0.000000000000000000 ) ) ;
#1373 = VECTOR ( 'NONE', #9662, 999.9999999999998863 ) ;
#1374 = CARTESIAN_POINT ( 'NONE',  ( 19.09188309203678813, 1.700000000000000178, -19.09188309203678813 ) ) ;
#1375 = CARTESIAN_POINT ( 'NONE',  ( 0.000000000000000000, 5.000000000000000000, 0.000000000000000000 ) ) ;
#1376 = ORIENTED_EDGE ( 'NONE', *, *, #1332, .T. ) ;
#1377 = ORIENTED_EDGE ( 'NONE', *, *, #9704, .F. ) ;
#1378 = CARTESIAN_POINT ( 'NONE',  ( -16.37951318544778445, 99.99999999999994316, 15.41600550949200077 ) ) ;
#1379 = CARTESIAN_POINT ( 'NONE',  ( -15.33577160963320374, 99.49999999999998579, 16.45272793336155814 ) ) ;
#1380 = VERTEX_POINT ( 'NONE', #8758 ) ;
#1381 = CARTESIAN_POINT ( 'NONE',  ( 2.256430356250000102, -4.978124999385482141, -2.763330213280484622E-16 ) ) ;
#1382 = ORIENTED_EDGE ( 'NONE', *, *, #8246, .F. ) ;
#1383 = VERTEX_POINT ( 'NONE', #7971 ) ;
#1384 = DIRECTION ( 'NONE',  ( -0.000000000000000000, 1.000000000000000000, -0.000000000000000000 ) ) ;
#1385 = CARTESIAN_POINT ( 'NONE',  ( 2.500000000000000444, -0.2625000000000000111, 1.443375672974063439 ) ) ;
#1386 = CARTESIAN_POINT ( 'NONE',  ( -2.256430356250000102, -0.7406249993854829849, -1.302750673588580321 ) ) ;
#1387 = CARTESIAN_POINT ( 'NONE',  ( 5.179363668139080445, 100.0000000000000995, -23.94265746362379943 ) ) ;
#1388 = CARTESIAN_POINT ( 'NONE',  ( 4.446585460023182890, 100.0000000000000000, -21.79057454014859019 ) ) ;
#1389 = ADVANCED_FACE ( 'NONE', ( #66 ), #9591, .T. ) ;
#1390 =( REPRESENTATION_RELATIONSHIP ('NONE','NONE', #3375, #5481 ) REPRESENTATION_RELATIONSHIP_WITH_TRANSFORMATION ( #7900 )SHAPE_REPRESENTATION_RELATIONSHIP( ) );
#1391 = CARTESIAN_POINT ( 'NONE',  ( 4.691018317478480526, 99.49999999999995737, -21.52316599815148024 ) ) ;
#1392 = VERTEX_POINT ( 'NONE', #7281 ) ;
#1393 = CARTESIAN_POINT ( 'NONE',  ( 3.375079225685456041, 99.50000000000000000, -22.79123997459842954 ) ) ;
#1394 = CARTESIAN_POINT ( 'NONE',  ( -0.2187216588148106211, -20.00000000000000000, -3.085264589354758336 ) ) ;
#1395 = ORIENTED_EDGE ( 'NONE', *, *, #843, .T. ) ;
#1396 =( GEOMETRIC_REPRESENTATION_CONTEXT ( 3 ) GLOBAL_UNCERTAINTY_ASSIGNED_CONTEXT ( ( #3296 ) ) GLOBAL_UNIT_ASSIGNED_CONTEXT ( ( #7429, #6752, #9893 ) ) REPRESENTATION_CONTEXT ( 'NONE', 'WORKASPACE' ) );
#1397 = PLANE ( 'NONE',  #7889 ) ;
#1398 = CARTESIAN_POINT ( 'NONE',  ( 2.256430356249999658, -1.678124999385482541, -1.302750673588581432 ) ) ;
#1399 = ORIENTED_EDGE ( 'NONE', *, *, #9313, .F. ) ;
#1400 = DIRECTION ( 'NONE',  ( -0.000000000000000000, -1.000000000000000000, -0.000000000000000000 ) ) ;
#1401 = CARTESIAN_POINT ( 'NONE',  ( 9.063633472794011325, 99.49999999999998579, 19.59517414759687526 ) ) ;
#1402 = EDGE_CURVE ( 'NONE', #4497, #84, #2382, .T. ) ;
#1403 = FACE_OUTER_BOUND ( 'NONE', #9984, .T. ) ;
#1404 = FACE_BOUND ( 'NONE', #10064, .T. ) ;
#1405 = ORIENTED_EDGE ( 'NONE', *, *, #1450, .F. ) ;
#1406 = CARTESIAN_POINT ( 'NONE',  ( -16.42071764973191250, 99.50000000000001421, 16.76105279315999042 ) ) ;
#1407 = CYLINDRICAL_SURFACE ( 'NONE', #5293, 2.500000000000000000 ) ;
#1408 = ORIENTED_EDGE ( 'NONE', *, *, #8045, .T. ) ;
#1409 = CARTESIAN_POINT ( 'NONE',  ( 2.500000000000000444, -2.962499999999999467, 1.443375672974063439 ) ) ;
#1410 = CARTESIAN_POINT ( 'NONE',  ( 1.045839947578414805E-15, -0.9562499987709659477, -2.500000000000000000 ) ) ;
#1411 = CARTESIAN_POINT ( 'NONE',  ( -2.256430356249999214, -2.915624999385482585, 1.302750673588581876 ) ) ;
#1412 = ADVANCED_FACE ( 'NONE', ( #2422 ), #8859, .T. ) ;
#1413 = CARTESIAN_POINT ( 'NONE',  ( -20.96643530928959365, 99.50000000000000000, -10.05541671241504886 ) ) ;
#1414 = CARTESIAN_POINT ( 'NONE',  ( -5.039362679103552881E-15, 1.749999998907525223, 27.43301270000000258 ) ) ;
#1415 = ORIENTED_EDGE ( 'NONE', *, *, #6754, .T. ) ;
#1416 = UNCERTAINTY_MEASURE_WITH_UNIT (LENGTH_MEASURE( 1.000000000000000082E-05 ), #8634, 'distance_accuracy_value', 'NONE');
#1417 = EDGE_CURVE ( 'NONE', #6040, #2765, #7542, .T. ) ;
#1418 = CARTESIAN_POINT ( 'NONE',  ( 9.164845778125666698, 100.0000000000000142, 19.62003801130714820 ) ) ;
#1419 = CARTESIAN_POINT ( 'NONE',  ( 3.673940397442059178E-15, 5.000000000000000000, 30.00000000000000000 ) ) ;
#1420 = CARTESIAN_POINT ( 'NONE',  ( 3.198738776810544415, 99.50000000000001421, -22.02447230026614022 ) ) ;
#1421 = PRODUCT_DEFINITION_SHAPE ( 'NONE', 'NONE',  #3149 ) ;
#1422 = CARTESIAN_POINT ( 'NONE',  ( -15.37731512048643268, 100.0000000000000000, 15.34394520743122214 ) ) ;
#1423 = ORIENTED_EDGE ( 'NONE', *, *, #2005, .T. ) ;
#1424 = CARTESIAN_POINT ( 'NONE',  ( 1.128215178125001161, -1.340624999385482852, 1.954126010382870815 ) ) ;
#1425 = CARTESIAN_POINT ( 'NONE',  ( 4.570993444255353921, 99.99999999999998579, -21.37574484917381668 ) ) ;
#1426 = ORIENTED_EDGE ( 'NONE', *, *, #10127, .F. ) ;
#1427 = CARTESIAN_POINT ( 'NONE',  ( 1.128215178125001161, -2.690624999385482941, 1.954126010382870815 ) ) ;
#1428 = CARTESIAN_POINT ( 'NONE',  ( 27.43301270000000258, 2.649999998907525356, 0.000000000000000000 ) ) ;
#1429 = CARTESIAN_POINT ( 'NONE',  ( 1.662111305799679408E-15, 5.083333332969175444, -27.14433756666667108 ) ) ;
#1430 = CARTESIAN_POINT ( 'NONE',  ( -11.18376618407356560, 0.2500000000000000000, -27.00000000000000355 ) ) ;
#1431 = CARTESIAN_POINT ( 'NONE',  ( 6.477538756577482459, 99.50000000000000000, 20.49684993083915430 ) ) ;
#1432 = ORIENTED_EDGE ( 'NONE', *, *, #294, .F. ) ;
#1433 = VECTOR ( 'NONE', #8642, 1000.000000000000000 ) ;
#1434 = CARTESIAN_POINT ( 'NONE',  ( 24.91446314102564230, 99.50000000000000000, -1.581029647435897578 ) ) ;
#1435 = CARTESIAN_POINT ( 'NONE',  ( 8.063732359723156051, 100.0000000000000142, 20.72384750152746236 ) ) ;
#1436 =( BOUNDED_CURVE ( )  B_SPLINE_CURVE ( 2, ( #817, #3322, #8871, #223, #2539, #3408, #4841, #5732, #7985 ),
 .UNSPECIFIED., .F., .T. ) 
 B_SPLINE_CURVE_WITH_KNOTS ( ( 3, 2, 2, 2, 3 ),
 ( 0.2500000000000000000, 0.2678571428571428492, 0.2857142857142856984, 0.3035714285714285476, 0.3214285714285714524 ),
 .UNSPECIFIED. ) 
 CURVE ( )  GEOMETRIC_REPRESENTATION_ITEM ( )  RATIONAL_B_SPLINE_CURVE ( ( 1.000000000000000000, 0.9238795325112867385, 1.000000000000000000, 0.9238795325112867385, 1.000000000000000000, 0.9238795325112867385, 1.000000000000000000, 0.9238795325112867385, 1.000000000000000000 ) ) 
 REPRESENTATION_ITEM ( '' )  );
#1437 = CARTESIAN_POINT ( 'NONE',  ( -1.595409442497313560E-16, -3.965624999385482408, -2.605501347177161087 ) ) ;
#1438 = VERTEX_POINT ( 'NONE', #8167 ) ;
#1439 = ORIENTED_EDGE ( 'NONE', *, *, #4589, .T. ) ;
#1440 = CARTESIAN_POINT ( 'NONE',  ( -15.72775836928289017, 100.0000000000000000, 17.03252426573849476 ) ) ;
#1441 = CARTESIAN_POINT ( 'NONE',  ( -21.00001322343447541, 99.50000000000001421, -9.990026185521596602 ) ) ;
#1442 = CARTESIAN_POINT ( 'NONE',  ( 4.786228327491940187E-16, -1.040624999385482807, 2.605501347177161087 ) ) ;
#1443 = CARTESIAN_POINT ( 'NONE',  ( -27.00000000000000355, 3.549999999999999822, -11.18376618407357270 ) ) ;
#1444 = VERTEX_POINT ( 'NONE', #1687 ) ;
#1445 = CARTESIAN_POINT ( 'NONE',  ( 3.681717055787076642, 100.0000000000000000, -21.09125273517263111 ) ) ;
#1446 = CARTESIAN_POINT ( 'NONE',  ( 1.249999999999999334, -2.793749998770965526, -2.165063509461096825 ) ) ;
#1447 = CARTESIAN_POINT ( 'NONE',  ( 3.058419780146050648, 99.50000000000000000, -23.12871267107006545 ) ) ;
#1448 = PLANE ( 'NONE',  #2297 ) ;
#1449 = ORIENTED_EDGE ( 'NONE', *, *, #6403, .T. ) ;
#1450 = EDGE_CURVE ( 'NONE', #6810, #8910, #1368, .T. ) ;
#1451 = CARTESIAN_POINT ( 'NONE',  ( 0.000000000000000000, 5.000000000000000000, 0.000000000000000000 ) ) ;
#1452 = CARTESIAN_POINT ( 'NONE',  ( 4.786228327491941173E-16, -1.378124999385482941, 2.605501347177161087 ) ) ;
#1453 = EDGE_CURVE ( 'NONE', #9675, #4732, #1321, .T. ) ;
#1454 = VERTEX_POINT ( 'NONE', #7421 ) ;
#1455 = PLANE ( 'NONE',  #93 ) ;
#1456 = AXIS2_PLACEMENT_3D ( 'NONE', #7770, #2109, #8615 ) ;
#1457 = PLANE ( 'NONE',  #33 ) ;
#1458 =( NAMED_UNIT ( * ) PLANE_ANGLE_UNIT ( ) SI_UNIT ( $, .RADIAN. ) );
#1459 = CARTESIAN_POINT ( 'NONE',  ( -0.6698729810778020211, -3.636153809338631415, -2.500000000000002665 ) ) ;
#1460 = ORIENTED_EDGE ( 'NONE', *, *, #3571, .T. ) ;
#1461 = DIRECTION ( 'NONE',  ( -1.000000000000000000, 0.000000000000000000, 1.224646799147352961E-16 ) ) ;
#1462 = VECTOR ( 'NONE', #7270, 1000.000000000000000 ) ;
#1463 = CARTESIAN_POINT ( 'NONE',  ( 9.182805720491336032, 100.0000000000000000, 20.00174565872165289 ) ) ;
#1464 = CARTESIAN_POINT ( 'NONE',  ( 2.500000000000000444, -3.412500000000000089, 1.443375672974063439 ) ) ;
#1465 = EDGE_CURVE ( 'NONE', #229, #7437, #3535, .T. ) ;
#1466 = CARTESIAN_POINT ( 'NONE',  ( 0.000000000000000000, 0.000000000000000000, -27.00000000000000000 ) ) ;
#1467 = CARTESIAN_POINT ( 'NONE',  ( 1.128215178125001161, -1.453124999385482896, 1.954126010382870815 ) ) ;
#1468 = CARTESIAN_POINT ( 'NONE',  ( 4.803433990161294354, 99.50000000000001421, -23.96838578116891583 ) ) ;
#1469 = CARTESIAN_POINT ( 'NONE',  ( -19.39806930854668465, 1.649999998907525356, 19.39806930854667755 ) ) ;
#1470 = VERTEX_POINT ( 'NONE', #4240 ) ;
#1471 = CARTESIAN_POINT ( 'NONE',  ( 1.250000000000001110, -2.100000000000000089, 2.165063509461096380 ) ) ;
#1472 = DIRECTION ( 'NONE',  ( 0.000000000000000000, -0.000000000000000000, -1.000000000000000000 ) ) ;
#1473 = CARTESIAN_POINT ( 'NONE',  ( 2.940631318607589417, 99.50000000000000000, -23.77584808773673331 ) ) ;
#1474 = CARTESIAN_POINT ( 'NONE',  ( 2.256430356250000546, -0.8531249993854829183, 1.302750673588579877 ) ) ;
#1475 = CARTESIAN_POINT ( 'NONE',  ( 3.948639947730041566, 99.49999999999998579, -21.07692942975820927 ) ) ;
#1476 = ORIENTED_EDGE ( 'NONE', *, *, #2750, .F. ) ;
#1477 = EDGE_CURVE ( 'NONE', #7818, #1371, #1027, .T. ) ;
#1478 = CARTESIAN_POINT ( 'NONE',  ( -1.128215178125000273, -1.115624999385482985, -1.954126010382871259 ) ) ;
#1479 = CARTESIAN_POINT ( 'NONE',  ( 11.36312591709336850, 3.299999998907525711, 27.43301269999999903 ) ) ;
#1480 = SURFACE_STYLE_FILL_AREA ( #62 ) ;
#1481 = CARTESIAN_POINT ( 'NONE',  ( 3.061616997868383043E-15, 100.0000000000000000, 25.00000000000000000 ) ) ;
#1482 = CARTESIAN_POINT ( 'NONE',  ( -4.959819536546781389E-15, 1.399999999999999911, 27.00000000000000355 ) ) ;
#1483 = VECTOR ( 'NONE', #6999, 1000.000000000000000 ) ;
#1484 = CARTESIAN_POINT ( 'NONE',  ( 8.612131858919537919, 99.49999999999998579, 19.96100069886393413 ) ) ;
#1485 = VERTEX_POINT ( 'NONE', #9202 ) ;
#1486 = CARTESIAN_POINT ( 'NONE',  ( -16.40919047799676989, 99.50000000000000000, 16.38364531277195013 ) ) ;
#1487 = CARTESIAN_POINT ( 'NONE',  ( 8.064245308217579122, 99.99999999999998579, 20.64099956338070641 ) ) ;
#1488 = EDGE_LOOP ( 'NONE', ( #2508, #3884 ) ) ;
#1489 = CARTESIAN_POINT ( 'NONE',  ( 1.128215178125001161, -5.053124999385482319, 1.954126010382870815 ) ) ;
#1490 = VERTEX_POINT ( 'NONE', #3450 ) ;
#1491 = CARTESIAN_POINT ( 'NONE',  ( 27.43301270000000258, 1.849999998907525534, 0.000000000000000000 ) ) ;
#1492 = LINE ( 'NONE', #4577, #6566 ) ;
#1493 = EDGE_CURVE ( 'NONE', #4732, #7023, #9993, .T. ) ;
#1494 = CARTESIAN_POINT ( 'NONE',  ( -2.256430356249998770, -2.015624999385482674, 1.302750673588581876 ) ) ;
#1495 = CARTESIAN_POINT ( 'NONE',  ( 5.226890989224467710, 99.50000000000000000, -23.72545275563321354 ) ) ;
#1496 = DIRECTION ( 'NONE',  ( 0.000000000000000000, 1.000000000000000000, 0.000000000000000000 ) ) ;
#1497 = EDGE_LOOP ( 'NONE', ( #1377, #2001, #3588, #479 ) ) ;
#1498 = CARTESIAN_POINT ( 'NONE',  ( -1.250000000000000222, -2.718749998770965792, -2.165063509461096825 ) ) ;
#1499 = CARTESIAN_POINT ( 'NONE',  ( 4.739008722453743161, 100.0000000000000142, -24.06821587619827341 ) ) ;
#1500 = CARTESIAN_POINT ( 'NONE',  ( 0.000000000000000000, 105.0000000000000142, -17.50000000000000355 ) ) ;
#1501 = ORIENTED_EDGE ( 'NONE', *, *, #10290, .F. ) ;
#1502 = CARTESIAN_POINT ( 'NONE',  ( 0.000000000000000000, 0.000000000000000000, 0.000000000000000000 ) ) ;
#1503 = CARTESIAN_POINT ( 'NONE',  ( -1.595409442497313560E-16, -2.053124999385482763, -2.605501347177161087 ) ) ;
#1504 = B_SPLINE_SURFACE_WITH_KNOTS ( 'NONE', 3, 1, ( 
 ( #10232, #7133 ),
 ( #2425, #4972 ),
 ( #8811, #2576 ),
 ( #9691, #5769 ),
 ( #8909, #1689 ),
 ( #6548, #1051 ),
 ( #7333, #2621 ),
 ( #6402, #3356 ),
 ( #5816, #68 ),
 ( #2531, #5724 ),
 ( #4193, #1640 ),
 ( #8172, #6594 ),
 ( #4885, #9784 ),
 ( #15, #168 ),
 ( #6455, #9005 ),
 ( #2479, #9644 ),
 ( #3313, #3217 ),
 ( #1000, #9738 ),
 ( #8125, #1826 ) ),
 .UNSPECIFIED., .F., .F., .F.,
 ( 4, 1, 1, 1, 1, 1, 1, 1, 1, 1, 1, 1, 1, 1, 1, 1, 4 ),
 ( 2, 2 ),
 ( 0.000000000000000000, 0.06455295689170470474, 0.1273249605695649933, 0.1891299628201091876, 0.2499617887110622549, 0.3104215510145779122, 0.3717966107350694216, 0.4346754705585744727, 0.4991966429079077727, 0.5636107885140392293, 0.6264421791528413941, 0.6882713145562978641, 0.7491215306807221808, 0.8100115732567139126, 0.8716292230916812267, 0.9349778748807419104, 1.000000000000000000 ),
 ( 0.000000000000000000, 1.000000000000000000 ),
 .UNSPECIFIED. ) ;
#1505 = CARTESIAN_POINT ( 'NONE',  ( 8.685676809262872666, 100.0000000000000000, 23.43455588346217766 ) ) ;
#1506 = CARTESIAN_POINT ( 'NONE',  ( 9.806436918512124734, 99.49999999999998579, 20.18080982695387604 ) ) ;
#1507 = DIRECTION ( 'NONE',  ( 0.000000000000000000, -1.000000000000000000, 0.000000000000000000 ) ) ;
#1508 = CARTESIAN_POINT ( 'NONE',  ( 9.877377282685029372E-16, -3.431249998770965259, 2.500000000000000000 ) ) ;
#1509 = ORIENTED_EDGE ( 'NONE', *, *, #310, .F. ) ;
#1510 = CARTESIAN_POINT ( 'NONE',  ( -19.09188309203678457, 2.499999997815050445, -19.09188309203678813 ) ) ;
#1511 = CARTESIAN_POINT ( 'NONE',  ( 1.679787559701184688E-15, 5.349999998907525089, -27.43301270000000258 ) ) ;
#1512 = ORIENTED_EDGE ( 'NONE', *, *, #4929, .T. ) ;
#1513 = CARTESIAN_POINT ( 'NONE',  ( 2.500000000000000000, -3.824999999999999734, -3.061616997868383141E-16 ) ) ;
#1514 = ITEM_DEFINED_TRANSFORMATION ( 'NONE', 'NONE', #8824,  #5055 ) ;
#1515 = CARTESIAN_POINT ( 'NONE',  ( 3.275092494823534928, 99.99999999999997158, -23.54688978826290580 ) ) ;
#1516 = CARTESIAN_POINT ( 'NONE',  ( -1.128215178124998497, -4.678124999385482319, 1.954126010382872147 ) ) ;
#1517 = CARTESIAN_POINT ( 'NONE',  ( 3.764204346677844093, 99.50000000000001421, -22.52576385118515745 ) ) ;
#1518 = CARTESIAN_POINT ( 'NONE',  ( 11.18376618407356915, 1.549999997815050490, -27.00000000000000355 ) ) ;
#1519 = CARTESIAN_POINT ( 'NONE',  ( -15.31787750341841559, 99.99999999999997158, 16.43551622900274722 ) ) ;
#1520 = CARTESIAN_POINT ( 'NONE',  ( 7.500000000000000000, 104.5000000000000142, 1.000000000000000222 ) ) ;
#1521 = CARTESIAN_POINT ( 'NONE',  ( 3.198592217420132666, 99.50000000000000000, -21.96964977087737836 ) ) ;
#1522 = EDGE_CURVE ( 'NONE', #7872, #10235, #289, .T. ) ;
#1523 = CARTESIAN_POINT ( 'NONE',  ( -22.67341330918043951, 100.0000000000000000, -10.57563951594260665 ) ) ;
#1524 = CARTESIAN_POINT ( 'NONE',  ( -1.128215178124998497, -3.215624999385482408, 1.954126010382872147 ) ) ;
#1525 = CARTESIAN_POINT ( 'NONE',  ( -20.74358258379034936, 99.49999999999998579, -9.818556592845180120 ) ) ;
#1526 = ORIENTED_EDGE ( 'NONE', *, *, #2961, .T. ) ;
#1527 = CARTESIAN_POINT ( 'NONE',  ( 2.256430356249999658, -3.028124999385482852, -1.302750673588581432 ) ) ;
#1528 = CARTESIAN_POINT ( 'NONE',  ( 1.679787559701184688E-15, 1.349999998907525312, -27.43301270000000258 ) ) ;
#1529 = CARTESIAN_POINT ( 'NONE',  ( -16.56926954694585774, 99.50000000000001421, 15.12296757606276643 ) ) ;
#1530 = LINE ( 'NONE', #6916, #2591 ) ;
#1531 = DIRECTION ( 'NONE',  ( 0.000000000000000000, 0.000000000000000000, -1.000000000000000000 ) ) ;
#1532 = DIRECTION ( 'NONE',  ( 0.000000000000000000, -1.000000000000000000, 0.000000000000000000 ) ) ;
#1533 = CARTESIAN_POINT ( 'NONE',  ( 8.231219904624582639, 100.0000000000000000, 20.21381436664452735 ) ) ;
#1534 = EDGE_LOOP ( 'NONE', ( #5350, #1415, #3867, #444 ) ) ;
#1535 = CARTESIAN_POINT ( 'NONE',  ( -2.256430356249999214, -5.165624999385481253, 1.302750673588581876 ) ) ;
#1536 = ORIENTED_EDGE ( 'NONE', *, *, #7153, .T. ) ;
#1537 = CARTESIAN_POINT ( 'NONE',  ( -19.39806930854668465, 1.549999998907525489, 19.39806930854667755 ) ) ;
#1538 = AXIS2_PLACEMENT_3D ( 'NONE', #3330, #9755, #7201 ) ;
#1539 = CARTESIAN_POINT ( 'NONE',  ( 3.977571997893210032, 99.50000000000000000, -24.70179182097838932 ) ) ;
#1540 = AXIS2_PLACEMENT_3D ( 'NONE', #7523, #2829, #6010 ) ;
#1541 = CARTESIAN_POINT ( 'NONE',  ( 2.500000000000000000, -1.125000000000000000, -3.061616997868383141E-16 ) ) ;
#1542 = CARTESIAN_POINT ( 'NONE',  ( -1.595409442497313560E-16, -1.265624999385482896, -2.605501347177161087 ) ) ;
#1543 = CARTESIAN_POINT ( 'NONE',  ( -2.562556682370380035, -20.00000000000000000, -1.479492790380212641 ) ) ;
#1544 = CARTESIAN_POINT ( 'NONE',  ( 9.834295043520187463, 100.0000000000000142, 21.14079655679390513 ) ) ;
#1545 = ORIENTED_EDGE ( 'NONE', *, *, #9344, .F. ) ;
#1546 = CARTESIAN_POINT ( 'NONE',  ( 0.000000000000000000, 75.00000000000001421, 0.000000000000000000 ) ) ;
#1547 = EDGE_CURVE ( 'NONE', #7571, #1061, #262, .T. ) ;
#1548 = VECTOR ( 'NONE', #7489, 1000.000000000000000 ) ;
#1549 = EDGE_CURVE ( 'NONE', #4027, #4436, #702, .T. ) ;
#1550 = ORIENTED_EDGE ( 'NONE', *, *, #4131, .T. ) ;
#1551 = CARTESIAN_POINT ( 'NONE',  ( 2.500000000000000000, -1.968749998770965792, -3.061616997868383141E-16 ) ) ;
#1552 = CARTESIAN_POINT ( 'NONE',  ( 2.500000000000000444, -1.106249998770965748, 1.443375672974063439 ) ) ;
#1553 = CARTESIAN_POINT ( 'NONE',  ( -1.249999999999998224, -3.074999999999999734, 2.165063509461097713 ) ) ;
#1554 = CARTESIAN_POINT ( 'NONE',  ( 8.465276868207817884, 99.50000000000001421, 19.66343818277063704 ) ) ;
#1555 = CARTESIAN_POINT ( 'NONE',  ( -1.128215178124998497, -4.565624999385482496, 1.954126010382872147 ) ) ;
#1556 = VECTOR ( 'NONE', #6322, 1000.000000000000000 ) ;
#1557 = ORIENTED_EDGE ( 'NONE', *, *, #9087, .T. ) ;
#1558 = CARTESIAN_POINT ( 'NONE',  ( 3.016803124593948393, 99.50000000000001421, -23.20507807535735978 ) ) ;
#1559 = FACE_OUTER_BOUND ( 'NONE', #5044, .T. ) ;
#1560 = CARTESIAN_POINT ( 'NONE',  ( -22.35673484330673944, 99.50000000000001421, -10.41320610523044721 ) ) ;
#1561 = DIRECTION ( 'NONE',  ( -0.05417351272771728926, 0.000000000000000000, -0.9985315370676781654 ) ) ;
#1562 = CARTESIAN_POINT ( 'NONE',  ( 19.39806930854667399, 5.049999998907525267, 19.39806930854668465 ) ) ;
#1563 = ORIENTED_EDGE ( 'NONE', *, *, #8450, .T. ) ;
#1564 = CARTESIAN_POINT ( 'NONE',  ( 1.250000000000001110, -4.799999999999999822, 2.165063509461096380 ) ) ;
#1565 = CONTEXT_DEPENDENT_SHAPE_REPRESENTATION ( #4800, #7671 ) ;
#1566 = CARTESIAN_POINT ( 'NONE',  ( 3.477525819554967423, 100.0000000000000000, -22.44236894434852658 ) ) ;
#1567 = CARTESIAN_POINT ( 'NONE',  ( -1.128215178124998497, -3.328124999385482230, 1.954126010382872147 ) ) ;
#1568 = CARTESIAN_POINT ( 'NONE',  ( -20.42657152723830905, 99.50000000000000000, -10.54129411626120216 ) ) ;
#1569 = CARTESIAN_POINT ( 'NONE',  ( -19.09188309203678457, 0.8999999978150503566, -19.09188309203678813 ) ) ;
#1570 =( GEOMETRIC_REPRESENTATION_CONTEXT ( 3 ) GLOBAL_UNCERTAINTY_ASSIGNED_CONTEXT ( ( #2145 ) ) GLOBAL_UNIT_ASSIGNED_CONTEXT ( ( #2268, #3164, #9494 ) ) REPRESENTATION_CONTEXT ( 'NONE', 'WORKASPACE' ) );
#1571 = LINE ( 'NONE', #3202, #100 ) ;
#1572 = CARTESIAN_POINT ( 'NONE',  ( 2.562556682370379146, -20.00000000000000000, -1.479492790380211975 ) ) ;
#1573 = CARTESIAN_POINT ( 'NONE',  ( 3.283294465904739390, 100.0000000000000284, -21.71066637097430885 ) ) ;
#1574 = CARTESIAN_POINT ( 'NONE',  ( 1.653273178848927064E-15, 4.200000000000000178, -27.00000000000000355 ) ) ;
#1575 = CARTESIAN_POINT ( 'NONE',  ( 1.128215178125001161, -4.040624999385483029, 1.954126010382870815 ) ) ;
#1576 = CARTESIAN_POINT ( 'NONE',  ( -21.30033281797529909, 99.50000000000002842, -9.345151174687854834 ) ) ;
#1577 = CARTESIAN_POINT ( 'NONE',  ( -2.256430356250000102, -3.290624999385482585, 0.000000000000000000 ) ) ;
#1578 = CARTESIAN_POINT ( 'NONE',  ( -19.39806930854667755, 1.449999998907525178, -19.39806930854668110 ) ) ;
#1579 = CARTESIAN_POINT ( 'NONE',  ( -15.58193289918752278, 99.50000000000000000, 16.98546238400348329 ) ) ;
#1580 = EDGE_CURVE ( 'NONE', #2567, #5889, #5964, .T. ) ;
#1581 = CARTESIAN_POINT ( 'NONE',  ( -11.36312591709335962, 0.4999999989075252227, -27.43301270000000258 ) ) ;
#1582 = DIRECTION ( 'NONE',  ( -0.9200099868272721970, 0.000000000000000000, 0.3918949146621865665 ) ) ;
#1583 = ORIENTED_EDGE ( 'NONE', *, *, #4726, .F. ) ;
#1584 = SHAPE_REPRESENTATION ( 'gas generator', ( #5055 ), #5746 ) ;
#1585 = SURFACE_STYLE_USAGE ( .BOTH. , #3216 ) ;
#1586 = CARTESIAN_POINT ( 'NONE',  ( 8.515772100368442565, 100.0000000000000000, 20.00046577258137503 ) ) ;
#1587 = ORIENTED_EDGE ( 'NONE', *, *, #6647, .T. ) ;
#1588 = CARTESIAN_POINT ( 'NONE',  ( 1.128215178124999607, -3.553124999385482319, -1.954126010382871259 ) ) ;
#1589 = ORIENTED_EDGE ( 'NONE', *, *, #5244, .F. ) ;
#1590 = CARTESIAN_POINT ( 'NONE',  ( 27.43301270000000258, 2.699999998907525178, -11.36312591709336139 ) ) ;
#1591 = DIRECTION ( 'NONE',  ( 0.000000000000000000, -1.000000000000000000, 0.000000000000000000 ) ) ;
#1592 = PRODUCT ( 'MAS-199', 'MAS-199', '', ( #7739 ) ) ;
#1593 = CARTESIAN_POINT ( 'NONE',  ( -21.84904385032055174, 99.99999999999998579, -11.42736543092427404 ) ) ;
#1594 = CARTESIAN_POINT ( 'NONE',  ( 1.128215178125001161, -4.153124999385482852, 1.954126010382870815 ) ) ;
#1595 = CARTESIAN_POINT ( 'NONE',  ( 10.72103337977569204, 99.50000000000000000, 22.20268488987243316 ) ) ;
#1596 = EDGE_CURVE ( 'NONE', #2682, #3764, #6034, .T. ) ;
#1597 = CARTESIAN_POINT ( 'NONE',  ( -16.92301558088953328, 99.50000000000001421, 15.88693424423437683 ) ) ;
#1598 = CARTESIAN_POINT ( 'NONE',  ( 8.399337394135656609, 99.99999999999998579, 20.06291166101774692 ) ) ;
#1599 = ADVANCED_FACE ( 'NONE', ( #3501 ), #6702, .F. ) ;
#1600 = CARTESIAN_POINT ( 'NONE',  ( 2.500000000000000000, -2.418749998770965526, -3.061616997868383141E-16 ) ) ;
#1601 = LINE ( 'NONE', #7991, #10153 ) ;
#1602 = DIRECTION ( 'NONE',  ( -0.8660254037844387076, 0.000000000000000000, 0.4999999999999997780 ) ) ;
#1604 = VECTOR ( 'NONE', #8608, 1000.000000000000000 ) ;
#1603 = CARTESIAN_POINT ( 'NONE',  ( -22.27115127098604574, 99.50000000000000000, -10.71048520281369676 ) ) ;
#1605 = CARTESIAN_POINT ( 'NONE',  ( 2.256430356249999658, -4.378124999385482496, -1.302750673588581432 ) ) ;
#1606 = EDGE_CURVE ( 'NONE', #10071, #1699, #2548, .T. ) ;
#1607 = CARTESIAN_POINT ( 'NONE',  ( 2.940631318607589417, 99.50000000000000000, -23.77584808773673331 ) ) ;
#1608 = ORIENTED_EDGE ( 'NONE', *, *, #2676, .T. ) ;
#1609 = EDGE_CURVE ( 'NONE', #5515, #10090, #5990, .T. ) ;
#1610 = CARTESIAN_POINT ( 'NONE',  ( 2.500000000000000444, -2.006249998770965437, 1.443375672974063439 ) ) ;
#1611 = CYLINDRICAL_SURFACE ( 'NONE', #6134, 27.00000000000000355 ) ;
#1612 = CARTESIAN_POINT ( 'NONE',  ( 19.39806930854668110, 3.649999998907525356, -19.39806930854668110 ) ) ;
#1613 = EDGE_LOOP ( 'NONE', ( #4097, #59 ) ) ;
#1614 = CARTESIAN_POINT ( 'NONE',  ( -2.500000000000000000, -4.500000000000000000, 0.000000000000000000 ) ) ;
#1615 = EDGE_CURVE ( 'NONE', #8551, #463, #1345, .T. ) ;
#1616 = VECTOR ( 'NONE', #3577, 999.9999999999998863 ) ;
#1617 = CARTESIAN_POINT ( 'NONE',  ( 3.328702480760086235, 99.99999999999994316, -23.35145716610488975 ) ) ;
#1618 = CARTESIAN_POINT ( 'NONE',  ( 2.256430356250000546, -4.115624999385482319, 1.302750673588579877 ) ) ;
#1619 = FACE_OUTER_BOUND ( 'NONE', #10298, .T. ) ;
#1620 = CARTESIAN_POINT ( 'NONE',  ( 1.653273178848927064E-15, 0.7999999978150503788, -27.00000000000000355 ) ) ;
#1621 = CARTESIAN_POINT ( 'NONE',  ( -20.64578974631102426, 99.99999999999995737, -10.10077944494247504 ) ) ;
#1622 = ORIENTED_EDGE ( 'NONE', *, *, #7157, .F. ) ;
#1623 = CLOSED_SHELL ( 'NONE', ( #5370, #3449, #10043, #5707, #9961, #3096, #3479, #7749, #3029, #8381, #5143, #705, #2732, #8657, #7497, #4346, #6568, #450, #263, #3444, #7268, #353, #7296, #4321, #7841, #5938, #9422, #2541, #516, #9883, #8829, #8223, #6008, #5300, #850, #6187, #1655, #8598, #9908, #4619, #9910, #1766, #7827 ) ) ;
#1624 = CARTESIAN_POINT ( 'NONE',  ( 3.478562133589548910, 99.49999999999997158, -24.13114810667639532 ) ) ;
#1625 = CARTESIAN_POINT ( 'NONE',  ( 3.399971579580567393, 100.0000000000000000, -21.57509867787664248 ) ) ;
#1626 = CARTESIAN_POINT ( 'NONE',  ( 11.18376618407357093, 4.150000000000000355, -27.00000000000000355 ) ) ;
#1627 = AXIS2_PLACEMENT_3D ( 'NONE', #8028, #9044, #4280 ) ;
#1628 = CARTESIAN_POINT ( 'NONE',  ( -1.128215178124998497, -2.765624999385482674, 1.954126010382872147 ) ) ;
#1629 = DIRECTION ( 'NONE',  ( -0.000000000000000000, 1.000000000000000000, -0.000000000000000000 ) ) ;
#1630 = EDGE_LOOP ( 'NONE', ( #3710, #125, #4256, #778 ) ) ;
#1631 = ORIENTED_EDGE ( 'NONE', *, *, #5530, .F. ) ;
#1632 = CARTESIAN_POINT ( 'NONE',  ( -1.128215178125000273, -3.365624999385482763, -1.954126010382871259 ) ) ;
#1633 = CARTESIAN_POINT ( 'NONE',  ( 11.36312591709336139, 5.199999998907525622, -27.43301270000000258 ) ) ;
#1634 = LINE ( 'NONE', #3212, #6445 ) ;
#1635 = CARTESIAN_POINT ( 'NONE',  ( 11.36312591709336850, 0.8999999989075253559, 27.43301269999999903 ) ) ;
#1636 = CARTESIAN_POINT ( 'NONE',  ( 3.028692941384139026, 99.50000000000001421, -22.52214499033115302 ) ) ;
#1637 = CARTESIAN_POINT ( 'NONE',  ( 3.000000000000000000, -15.00000000000000000, 1.732050807568879192 ) ) ;
#1638 = EDGE_LOOP ( 'NONE', ( #10223, #2329, #1348, #5031 ) ) ;
#1639 = ADVANCED_BREP_SHAPE_REPRESENTATION ( '', ( #3102, #5055 ), #3636 ) ;
#1640 = CARTESIAN_POINT ( 'NONE',  ( -20.96129225301843135, 99.99999999999998579, -10.68089388303413934 ) ) ;
#1641 = EDGE_CURVE ( 'NONE', #827, #2600, #3703, .T. ) ;
#1642 = FACE_OUTER_BOUND ( 'NONE', #3861, .T. ) ;
#1643 = ORIENTED_EDGE ( 'NONE', *, *, #8965, .F. ) ;
#1644 = CARTESIAN_POINT ( 'NONE',  ( -19.39806930854668465, 3.149999998907525356, 19.39806930854667755 ) ) ;
#1645 = CARTESIAN_POINT ( 'NONE',  ( 2.940631318607589417, 100.0000000000000000, -23.77584808773673331 ) ) ;
#1646 = FACE_OUTER_BOUND ( 'NONE', #2819, .T. ) ;
#1647 =( GEOMETRIC_REPRESENTATION_CONTEXT ( 3 ) GLOBAL_UNCERTAINTY_ASSIGNED_CONTEXT ( ( #7169 ) ) GLOBAL_UNIT_ASSIGNED_CONTEXT ( ( #1688, #4831, #7184 ) ) REPRESENTATION_CONTEXT ( 'NONE', 'WORKASPACE' ) );
#1648 = CARTESIAN_POINT ( 'NONE',  ( -2.256430356250000102, -3.853124999385482585, 0.000000000000000000 ) ) ;
#1649 = DIRECTION ( 'NONE',  ( 0.000000000000000000, 0.000000000000000000, -1.000000000000000000 ) ) ;
#1650 = CARTESIAN_POINT ( 'NONE',  ( -16.90147242988460263, 99.99999999999998579, 15.68472263728856753 ) ) ;
#1651 =( BOUNDED_CURVE ( )  B_SPLINE_CURVE ( 2, ( #1508, #5545, #8636, #95, #3920, #7205, #9522, #1459, #37 ),
 .UNSPECIFIED., .F., .F. ) 
 B_SPLINE_CURVE_WITH_KNOTS ( ( 3, 2, 2, 2, 3 ),
 ( 0.5625000000000000000, 0.5694444444444444198, 0.5833333333333333703, 0.5972222222222222099, 0.6041666666666667407 ),
 .UNSPECIFIED. ) 
 CURVE ( )  GEOMETRIC_REPRESENTATION_ITEM ( )  RATIONAL_B_SPLINE_CURVE ( ( 0.9330127018922194093, 0.9330127018922194093, 1.000000000000000000, 0.8660254037844387076, 1.000000000000000000, 0.8660254037844387076, 1.000000000000000000, 0.9330127018922187432, 0.9330127018922192983 ) ) 
 REPRESENTATION_ITEM ( '' )  );
#1652 = EDGE_LOOP ( 'NONE', ( #6054, #6847, #8487, #1948 ) ) ;
#1653 = AXIS2_PLACEMENT_3D ( 'NONE', #458, #3760, #4535 ) ;
#1654 = CARTESIAN_POINT ( 'NONE',  ( -1.767625397874844694E-16, -1.856249998770965526, -2.886751345948128655 ) ) ;
#1655 = ADVANCED_FACE ( 'NONE', ( #2813, #3864 ), #10084, .T. ) ;
#1656 = CARTESIAN_POINT ( 'NONE',  ( 4.743081672682207817, 100.0000000000000284, -21.60795120912350598 ) ) ;
#1657 = FACE_BOUND ( 'NONE', #8386, .T. ) ;
#1658 = CARTESIAN_POINT ( 'NONE',  ( 9.526349065647009340, 99.50000000000000000, 19.81320455978211470 ) ) ;
#1659 = CARTESIAN_POINT ( 'NONE',  ( -1.595409442497313560E-16, -4.303124999385482319, -2.605501347177161087 ) ) ;
#1660 = EDGE_LOOP ( 'NONE', ( #8586, #567, #5060, #187 ) ) ;
#1661 = DIRECTION ( 'NONE',  ( -0.000000000000000000, 1.000000000000000000, -0.000000000000000000 ) ) ;
#1662 = PRESENTATION_STYLE_ASSIGNMENT (( #8834 ) ) ;
#1663 = CARTESIAN_POINT ( 'NONE',  ( -9.703070624755296135E-15, -3.487499999999999822, 2.500000000000000444 ) ) ;
#1664 = CARTESIAN_POINT ( 'NONE',  ( 24.93339342948717885, 99.50000000000000000, -1.235376602564102644 ) ) ;
#1665 = CARTESIAN_POINT ( 'NONE',  ( 8.973011566395204142, 99.99999999999997158, 19.93291184930431115 ) ) ;
#1666 = ORIENTED_EDGE ( 'NONE', *, *, #5442, .F. ) ;
#1667 = B_SPLINE_CURVE_WITH_KNOTS ( 'NONE', 3,
 ( #331, #7438, #3522, #8187, #8975, #4257, #5034, #5736, #1117, #9022, #3326, #6659, #1015, #2638, #6707 ),
 .UNSPECIFIED., .F., .F.,
 ( 4, 1, 1, 1, 1, 1, 1, 1, 1, 1, 1, 1, 4 ),
 ( 0.000000000000000000, 0.08450893420292937552, 0.1670077533940913517, 0.2489527561816328172, 0.3323249201989921797, 0.4152786837838207679, 0.4972150204155297848, 0.5791806016509544186, 0.6636863847498374325, 0.7483757861910059761, 0.8320455266939520422, 0.9153409992114193150, 1.000000000000000000 ),
 .UNSPECIFIED. ) ;
#1668 = CARTESIAN_POINT ( 'NONE',  ( 3.080354370726382296, 99.50000000000004263, -23.09295995363041598 ) ) ;
#1669 = FACE_OUTER_BOUND ( 'NONE', #10289, .T. ) ;
#1670 = CARTESIAN_POINT ( 'NONE',  ( 2.256430356249999658, -4.940624999385482496, -1.302750673588581432 ) ) ;
#1671 = CARTESIAN_POINT ( 'NONE',  ( -20.89169796687544789, 99.50000000000001421, -10.40078880447404330 ) ) ;
#1672 = CARTESIAN_POINT ( 'NONE',  ( -19.09188309203678457, 1.699999997815050401, -19.09188309203678813 ) ) ;
#1673 = ADVANCED_FACE ( 'NONE', ( #5207 ), #1457, .F. ) ;
#1674 = CARTESIAN_POINT ( 'NONE',  ( -15.32348647777738826, 99.50000000000000000, 15.39505148541300450 ) ) ;
#1675 = DIRECTION ( 'NONE',  ( 0.000000000000000000, 0.000000000000000000, -1.000000000000000000 ) ) ;
#1676 = CARTESIAN_POINT ( 'NONE',  ( 3.202955020264580899, 100.0000000000000000, -21.91595956354277064 ) ) ;
#1677 = B_SPLINE_SURFACE_WITH_KNOTS ( 'NONE', 3, 1, ( 
 ( #7079, #7867 ),
 ( #7919, #646 ),
 ( #7817, #7706 ),
 ( #2160, #6135 ),
 ( #9498, #3841 ),
 ( #2272, #9386 ),
 ( #5521, #9329 ),
 ( #10284, #2895 ),
 ( #7763, #3061 ),
 ( #4625, #6244 ),
 ( #7026, #5470 ),
 ( #1323, #542 ),
 ( #10229, #5361 ),
 ( #6300, #2322 ),
 ( #9444, #2103 ),
 ( #8550, #3735 ),
 ( #1484, #2215 ),
 ( #4678, #6917 ),
 ( #697, #5418 ) ),
 .UNSPECIFIED., .F., .F., .F.,
 ( 4, 1, 1, 1, 1, 1, 1, 1, 1, 1, 1, 1, 1, 1, 1, 1, 4 ),
 ( 2, 2 ),
 ( 0.000000000000000000, 0.06222907146265880401, 0.1227741760084055250, 0.1821991178386986321, 0.2415152369242211383, 0.3014228132391471027, 0.3622599083280184651, 0.4248173832850619669, 0.4890434280230284148, 0.5537961591902206271, 0.6173286602167864512, 0.6798064121185800612, 0.7417947397634444551, 0.8039614856828293243, 0.8674939867093949264, 0.9325113003366737319, 1.000000000000000000 ),
 ( 0.000000000000000000, 1.000000000000000000 ),
 .UNSPECIFIED. ) ;
#1678 = ADVANCED_FACE ( 'NONE', ( #2009 ), #7944, .T. ) ;
#1679 = CARTESIAN_POINT ( 'NONE',  ( -22.57971655928959365, 100.0000000000000000, -10.84768434062017839 ) ) ;
#1680 = CARTESIAN_POINT ( 'NONE',  ( 4.786228327491940187E-16, -3.178124999385483207, 2.605501347177161087 ) ) ;
#1681 = DIRECTION ( 'NONE',  ( 0.000000000000000000, 1.000000000000000000, 0.000000000000000000 ) ) ;
#1682 = ORIENTED_EDGE ( 'NONE', *, *, #8100, .T. ) ;
#1683 = CARTESIAN_POINT ( 'NONE',  ( -2.500000000000000000, -0.4874999999999999334, -1.443375672974064106 ) ) ;
#1684 = CARTESIAN_POINT ( 'NONE',  ( -27.43301270000000969, 4.699999998907524734, 11.36312591709335429 ) ) ;
#1685 = DIRECTION ( 'NONE',  ( 0.000000000000000000, -1.000000000000000000, 0.000000000000000000 ) ) ;
#1686 = CARTESIAN_POINT ( 'NONE',  ( 27.00000000000000355, 3.250000000000000444, -11.18376618407356737 ) ) ;
#1687 = CARTESIAN_POINT ( 'NONE',  ( -1.915118561403101438, -5.394273269507307234, -1.606960141313192203 ) ) ;
#1688 =( LENGTH_UNIT ( ) NAMED_UNIT ( * ) SI_UNIT ( .MILLI., .METRE. ) );
#1689 = CARTESIAN_POINT ( 'NONE',  ( -20.89948324804827706, 99.99999999999998579, -10.26098411820691858 ) ) ;
#1690 = CARTESIAN_POINT ( 'NONE',  ( -20.74358258379034936, 99.49999999999998579, -9.818556592845180120 ) ) ;
#1691 = CARTESIAN_POINT ( 'NONE',  ( 19.39806930854668110, 2.749999998907525001, -19.39806930854668110 ) ) ;
#1692 = CARTESIAN_POINT ( 'NONE',  ( 3.293272160652527258, 99.99999999999997158, -24.41359064397622802 ) ) ;
#1693 = CARTESIAN_POINT ( 'NONE',  ( 0.6698729810778063509, -1.032596189432334111, -2.500000000000000000 ) ) ;
#1694 = CARTESIAN_POINT ( 'NONE',  ( 2.256430356250000102, -4.528124999385481964, -2.763330213280484622E-16 ) ) ;
#1695 = CARTESIAN_POINT ( 'NONE',  ( -16.45391695211397831, 100.0000000000000426, 16.32580124622701589 ) ) ;
#1696 = CARTESIAN_POINT ( 'NONE',  ( -16.91946509138130139, 100.0000000000000142, 15.98858002463268413 ) ) ;
#1697 = CARTESIAN_POINT ( 'NONE',  ( 5.242860087038358152, 100.0000000000000284, -23.52699316036146371 ) ) ;
#1698 = CARTESIAN_POINT ( 'NONE',  ( 2.500000000000000444, -4.256249998770965881, 1.443375672974063439 ) ) ;
#1699 = VERTEX_POINT ( 'NONE', #8165 ) ;
#1700 = CARTESIAN_POINT ( 'NONE',  ( -22.31230063665282515, 99.49999999999997158, -10.62159318200525249 ) ) ;
#1701 = CARTESIAN_POINT ( 'NONE',  ( -15.24337324910153946, 99.49999999999997158, 16.81353386054630761 ) ) ;
#1702 = CARTESIAN_POINT ( 'NONE',  ( -2.500000000000000000, 0.000000000000000000, 0.000000000000000000 ) ) ;
#1703 = CARTESIAN_POINT ( 'NONE',  ( 2.256430356250000102, -3.515624999385482674, -2.763330213280484622E-16 ) ) ;
#1704 = AXIS2_PLACEMENT_3D ( 'NONE', #8807, #9734, #5767 ) ;
#1705 = EDGE_CURVE ( 'NONE', #7134, #10177, #7370, .T. ) ;
#1706 = ORIENTED_EDGE ( 'NONE', *, *, #8873, .T. ) ;
#1707 = B_SPLINE_CURVE_WITH_KNOTS ( 'NONE', 3,
 ( #8049, #3975, #884, #7159, #9670, #2453, #4074, #97, #1463, #5649, #8838, #1665, #4859, #3289, #3869, #9714, #7309, #6525, #2555 ),
 .UNSPECIFIED., .F., .F.,
 ( 4, 1, 1, 1, 1, 1, 1, 1, 1, 1, 1, 1, 1, 1, 1, 1, 4 ),
 ( 0.000000000000000000, 0.06222907146265880401, 0.1227741760084055250, 0.1821991178386986321, 0.2415152369242211383, 0.3014228132391471027, 0.3622599083280184651, 0.4248173832850619669, 0.4890434280230284148, 0.5537961591902206271, 0.6173286602167864512, 0.6798064121185800612, 0.7417947397634444551, 0.8039614856828293243, 0.8674939867093949264, 0.9325113003366737319, 1.000000000000000000 ),
 .UNSPECIFIED. ) ;
#1708 = CARTESIAN_POINT ( 'NONE',  ( 27.00000000000000355, 0.2999999989075251561, 0.000000000000000000 ) ) ;
#1709 = DIRECTION ( 'NONE',  ( 0.000000000000000000, -0.000000000000000000, 1.000000000000000000 ) ) ;
#1710 = LINE ( 'NONE', #10308, #9489 ) ;
#1711 = CARTESIAN_POINT ( 'NONE',  ( 1.653273178848927064E-15, 4.200000000000000178, -27.00000000000000355 ) ) ;
#1712 = AXIS2_PLACEMENT_3D ( 'NONE', #3630, #6920, #6811 ) ;
#1713 = VERTEX_POINT ( 'NONE', #260 ) ;
#1714 = CARTESIAN_POINT ( 'NONE',  ( -21.18296228862668329, 100.0000000000000284, -10.95406920104765724 ) ) ;
#1715 = CARTESIAN_POINT ( 'NONE',  ( -1.595409442497313560E-16, -0.2531249993854829405, -2.605501347177161087 ) ) ;
#1716 = EDGE_CURVE ( 'NONE', #4040, #10122, #5117, .T. ) ;
#1717 = EDGE_LOOP ( 'NONE', ( #8594, #6345, #1476, #878 ) ) ;
#1718 = CARTESIAN_POINT ( 'NONE',  ( 3.986298408513477387, 99.50000000000002842, -22.53092616755505162 ) ) ;
#1719 = CARTESIAN_POINT ( 'NONE',  ( -11.18376618407356560, 0.8499999978150503122, -27.00000000000000355 ) ) ;
#1720 = AXIS2_PLACEMENT_3D ( 'NONE', #9929, #1813, #4230 ) ;
#1721 = DIRECTION ( 'NONE',  ( -0.5137073458062109133, 0.000000000000000000, -0.8579654788304353907 ) ) ;
#1722 = AXIS2_PLACEMENT_3D ( 'NONE', #10052, #6803, #8544 ) ;
#1723 = CARTESIAN_POINT ( 'NONE',  ( -4.959819536546781389E-15, 3.599999997815050534, 27.00000000000000355 ) ) ;
#1724 = CARTESIAN_POINT ( 'NONE',  ( 3.717146347979291665, 100.0000000000000000, -21.42716062222556417 ) ) ;
#1725 = CARTESIAN_POINT ( 'NONE',  ( 5.243816414761435674, 100.0000000000000000, -23.48558366465980995 ) ) ;
#1726 = CARTESIAN_POINT ( 'NONE',  ( 2.256430356249999658, -2.578124999385483118, -1.302750673588581432 ) ) ;
#1727 = ORIENTED_EDGE ( 'NONE', *, *, #7157, .T. ) ;
#1728 = CARTESIAN_POINT ( 'NONE',  ( -1.595409442497313560E-16, -3.853124999385482585, -2.605501347177161087 ) ) ;
#1729 = ADVANCED_FACE ( 'NONE', ( #1972 ), #5608, .T. ) ;
#1730 = CARTESIAN_POINT ( 'NONE',  ( -15.70584307919286893, 99.50000000000000000, 14.84247401567675162 ) ) ;
#1731 = EDGE_CURVE ( 'NONE', #7666, #2013, #1770, .T. ) ;
#1732 = CARTESIAN_POINT ( 'NONE',  ( -19.39806930854667755, 0.5499999989075252671, -19.39806930854668110 ) ) ;
#1733 = CARTESIAN_POINT ( 'NONE',  ( 2.912748042341355870, 99.99999999999998579, -22.34826719014139940 ) ) ;
#1734 = CARTESIAN_POINT ( 'NONE',  ( 27.00000000000000355, 2.199999997815050623, 0.000000000000000000 ) ) ;
#1735 = ORIENTED_EDGE ( 'NONE', *, *, #5028, .F. ) ;
#1736 = CARTESIAN_POINT ( 'NONE',  ( 4.241330131419338123, 99.99999999999998579, -24.68798891778770965 ) ) ;
#1737 = DIRECTION ( 'NONE',  ( 0.000000000000000000, 0.000000000000000000, -1.000000000000000000 ) ) ;
#1738 = CARTESIAN_POINT ( 'NONE',  ( -1.128215178125000273, -3.928124999385483207, -1.954126010382871259 ) ) ;
#1739 = CARTESIAN_POINT ( 'NONE',  ( 4.232798786556307036, 100.0000000000000000, -24.34936571594186105 ) ) ;
#1740 = CARTESIAN_POINT ( 'NONE',  ( -22.08823018108446234, 100.0000000000000000, -9.406177930363766038 ) ) ;
#1741 = CARTESIAN_POINT ( 'NONE',  ( 8.067960508813904141, 100.0000000000000000, 20.80952186068213905 ) ) ;
#1742 = CARTESIAN_POINT ( 'NONE',  ( 1.250000000000001110, -5.193749998770964993, 2.165063509461096380 ) ) ;
#1743 = ORIENTED_EDGE ( 'NONE', *, *, #8141, .F. ) ;
#1744 = ORIENTED_EDGE ( 'NONE', *, *, #6056, .T. ) ;
#1745 = CARTESIAN_POINT ( 'NONE',  ( 0.000000000000000000, 0.000000000000000000, -2.500000000000000000 ) ) ;
#1746 = CARTESIAN_POINT ( 'NONE',  ( 3.283294465904739390, 99.50000000000002842, -21.71066637097430885 ) ) ;
#1747 = CARTESIAN_POINT ( 'NONE',  ( -21.99951964646687941, 99.50000000000001421, -11.00094659099690553 ) ) ;
#1748 = CARTESIAN_POINT ( 'NONE',  ( -1.128215178124998497, -5.015624999385482674, 1.954126010382872147 ) ) ;
#1749 = ORIENTED_EDGE ( 'NONE', *, *, #5688, .T. ) ;
#1750 = DIRECTION ( 'NONE',  ( -1.000000000000000000, 1.320207234900709352E-11, 0.000000000000000000 ) ) ;
#1751 = CARTESIAN_POINT ( 'NONE',  ( -0.6698729810778069060, -3.692403810567665978, -2.500000000000000000 ) ) ;
#1752 = EDGE_CURVE ( 'NONE', #5272, #4302, #8212, .T. ) ;
#1753 = CARTESIAN_POINT ( 'NONE',  ( -7.500000000000000000, 104.5000000000000142, -3.000000000000000000 ) ) ;
#1754 =( BOUNDED_CURVE ( )  B_SPLINE_CURVE ( 2, ( #5225, #4498, #7691, #6904, #2146, #10099, #1471, #4868, #9629 ),
 .UNSPECIFIED., .F., .T. ) 
 B_SPLINE_CURVE_WITH_KNOTS ( ( 3, 2, 2, 2, 3 ),
 ( 0.3541666666666666852, 0.3611111111111111049, 0.3750000000000000000, 0.3888888888888888951, 0.3958333333333333703 ),
 .UNSPECIFIED. ) 
 CURVE ( )  GEOMETRIC_REPRESENTATION_ITEM ( )  RATIONAL_B_SPLINE_CURVE ( ( 0.9330127018922194093, 0.9330127018922196314, 1.000000000000000000, 0.8660254037844387076, 1.000000000000000000, 0.8660254037844387076, 1.000000000000000000, 0.9330127018922190762, 0.9330127018922194093 ) ) 
 REPRESENTATION_ITEM ( '' )  );
#1755 = ADVANCED_FACE ( 'NONE', ( #1044 ), #4967, .T. ) ;
#1756 = CARTESIAN_POINT ( 'NONE',  ( 3.374624233514611937, 100.0000000000000000, -23.25900349070959550 ) ) ;
#1757 = CARTESIAN_POINT ( 'NONE',  ( 3.739209042966564311, 99.50000000000001421, -21.42288334414699591 ) ) ;
#1758 = CARTESIAN_POINT ( 'NONE',  ( 3.195700652717397894, 99.49999999999997158, -22.66286045753255962 ) ) ;
#1759 = CARTESIAN_POINT ( 'NONE',  ( 19.09188309203678102, 5.299999997815050712, 19.09188309203678813 ) ) ;
#1760 = CARTESIAN_POINT ( 'NONE',  ( -20.72805389903318130, 99.50000000000000000, -9.848585782927868237 ) ) ;
#1761 = LINE ( 'NONE', #9094, #8320 ) ;
#1762 = CARTESIAN_POINT ( 'NONE',  ( 3.497829868842083023, 100.0000000000000000, -21.50512556757917793 ) ) ;
#1763 = CARTESIAN_POINT ( 'NONE',  ( -22.27115127098604574, 100.0000000000000000, -10.71048520281369676 ) ) ;
#1764 = DIRECTION ( 'NONE',  ( -0.000000000000000000, -1.000000000000000000, -0.000000000000000000 ) ) ;
#1765 = EDGE_CURVE ( 'NONE', #8002, #10148, #10057, .T. ) ;
#1766 = ADVANCED_FACE ( 'NONE', ( #1922 ), #5239, .T. ) ;
#1767 = CIRCLE ( 'NONE', #1936, 24.00000000000000355 ) ;
#1768 = CARTESIAN_POINT ( 'NONE',  ( 2.256430356250000546, -4.903124999385481964, 1.302750673588579877 ) ) ;
#1769 = PLANE ( 'NONE',  #7599 ) ;
#1770 = LINE ( 'NONE', #9050, #5729 ) ;
#1771 = CARTESIAN_POINT ( 'NONE',  ( -19.09188309203678457, 4.299999999999999822, -19.09188309203678813 ) ) ;
#1772 = CARTESIAN_POINT ( 'NONE',  ( -7.500000000000000000, 105.0000000000000142, 1.000000000000000222 ) ) ;
#1773 = CARTESIAN_POINT ( 'NONE',  ( -20.69312081029678296, 99.99999999999997158, -9.926742041671966277 ) ) ;
#1774 = AXIS2_PLACEMENT_3D ( 'NONE', #2910, #8507, #3030 ) ;
#1775 = FACE_OUTER_BOUND ( 'NONE', #6727, .T. ) ;
#1776 = CARTESIAN_POINT ( 'NONE',  ( 21.43339342948717885, 100.0000000000000000, -1.392427884615384803 ) ) ;
#1777 = VERTEX_POINT ( 'NONE', #5037 ) ;
#1778 = ORIENTED_EDGE ( 'NONE', *, *, #7012, .F. ) ;
#1779 = CARTESIAN_POINT ( 'NONE',  ( 8.223467485077383898, 99.49999999999997158, 19.78581333328655134 ) ) ;
#1780 = CLOSED_SHELL ( 'NONE', ( #7325, #8365, #5184, #7203 ) ) ;
#1781 = DIRECTION ( 'NONE',  ( 0.3918949146621865109, 0.000000000000000000, 0.9200099868272720860 ) ) ;
#1782 = CARTESIAN_POINT ( 'NONE',  ( -21.94169572595625795, 99.50000000000000000, -9.715372641902229489 ) ) ;
#1783 = CARTESIAN_POINT ( 'NONE',  ( -21.20999280589743918, 100.0000000000000284, -11.35389291771566000 ) ) ;
#1784 = CARTESIAN_POINT ( 'NONE',  ( 2.256430356250000102, -3.178124999385482319, -2.763330213280484622E-16 ) ) ;
#1785 = CARTESIAN_POINT ( 'NONE',  ( 0.6698729810778087934, -2.326346188203300525, -2.499999999999999112 ) ) ;
#1786 = CARTESIAN_POINT ( 'NONE',  ( -22.33111803333905243, 99.49999999999997158, -9.558150950182401573 ) ) ;
#1787 = CARTESIAN_POINT ( 'NONE',  ( -0.6698729810778043525, -1.892403810567665712, -2.500000000000001332 ) ) ;
#1788 = ORIENTED_EDGE ( 'NONE', *, *, #3153, .T. ) ;
#1789 = CARTESIAN_POINT ( 'NONE',  ( 2.500000000000000000, -3.731249998770965970, -1.443375672974064994 ) ) ;
#1790 = VERTEX_POINT ( 'NONE', #9805 ) ;
#1791 = ORIENTED_EDGE ( 'NONE', *, *, #2551, .T. ) ;
#1792 = EDGE_CURVE ( 'NONE', #5243, #3042, #5518, .T. ) ;
#1793 = AXIS2_PLACEMENT_3D ( 'NONE', #8217, #9836, #2575 ) ;
#1794 = DIRECTION ( 'NONE',  ( 0.000000000000000000, 1.000000000000000000, 0.000000000000000000 ) ) ;
#1795 = CARTESIAN_POINT ( 'NONE',  ( 3.198592217420132666, 99.99999999999997158, -21.96964977087737836 ) ) ;
#1796 = CARTESIAN_POINT ( 'NONE',  ( -14.89508182811745662, 99.99999999999997158, 15.38112983991209326 ) ) ;
#1797 = CARTESIAN_POINT ( 'NONE',  ( 4.688812652749139609, 100.0000000000000426, -24.54863390154074310 ) ) ;
#1798 = ORIENTED_EDGE ( 'NONE', *, *, #3264, .T. ) ;
#1799 = CIRCLE ( 'NONE', #7161, 2.500000000000000000 ) ;
#1800 = DIRECTION ( 'NONE',  ( -0.000000000000000000, 1.000000000000000000, -0.000000000000000000 ) ) ;
#1801 = LINE ( 'NONE', #6571, #2147 ) ;
#1802 = FACE_OUTER_BOUND ( 'NONE', #2622, .T. ) ;
#1803 = ORIENTED_EDGE ( 'NONE', *, *, #651, .T. ) ;
#1804 = B_SPLINE_CURVE_WITH_KNOTS ( 'NONE', 3,
 ( #8597, #8700, #1420, #1521, #4609, #3158, #7802, #633, #3831, #8649, #6232, #9433, #4715, #7908, #6341, #9535, #4500, #157, #9631 ),
 .UNSPECIFIED., .F., .F.,
 ( 4, 1, 1, 1, 1, 1, 1, 1, 1, 1, 1, 1, 1, 1, 1, 1, 4 ),
 ( 0.000000000000000000, 0.05935611633690887623, 0.1167563879513689451, 0.1743885027374874330, 0.2308223543163396840, 0.2888100779544915953, 0.3475404098195560842, 0.4086537266250744316, 0.4723446836969566465, 0.5362968130936018873, 0.6000923674009760456, 0.6637702377379335328, 0.7274568328636339398, 0.7924602533659969028, 0.8590386936388050287, 0.9283644560612371865, 1.000000000000000000 ),
 .UNSPECIFIED. ) ;
#1805 = CYLINDRICAL_SURFACE ( 'NONE', #3738, 27.00000000000000355 ) ;
#1806 = CARTESIAN_POINT ( 'NONE',  ( 3.409892249890944527, 99.50000000000000000, -24.50637943905448779 ) ) ;
#1807 = CARTESIAN_POINT ( 'NONE',  ( 7.746148141271532950, 99.99999999999997158, 20.51930889200067298 ) ) ;
#1808 = VERTEX_POINT ( 'NONE', #1170 ) ;
#1809 = CARTESIAN_POINT ( 'NONE',  ( 3.477525819554967423, 99.50000000000000000, -22.44236894434852658 ) ) ;
#1810 = CARTESIAN_POINT ( 'NONE',  ( 19.09188309203678813, 3.899999997815050357, -19.09188309203678813 ) ) ;
#1811 = CARTESIAN_POINT ( 'NONE',  ( -20.72805389903318130, 100.0000000000000000, -9.848585782927868237 ) ) ;
#1812 = CARTESIAN_POINT ( 'NONE',  ( -21.80427673524616239, 100.0000000000000000, -9.663674634844889866 ) ) ;
#1813 = DIRECTION ( 'NONE',  ( 0.000000000000000000, -1.000000000000000000, 0.000000000000000000 ) ) ;
#1814 = CARTESIAN_POINT ( 'NONE',  ( -21.51485068221570174, 99.50000000000000000, -11.09552232883975087 ) ) ;
#1815 = CARTESIAN_POINT ( 'NONE',  ( 0.000000000000000000, -25.00000000000000000, 0.000000000000000000 ) ) ;
#1816 = CARTESIAN_POINT ( 'NONE',  ( -4.959819536546781389E-15, 4.399999997815050357, 27.00000000000000355 ) ) ;
#1817 = CARTESIAN_POINT ( 'NONE',  ( 4.786228327491941173E-16, -4.978124999385483029, 2.605501347177161087 ) ) ;
#1818 = SHAPE_REPRESENTATION_RELATIONSHIP ( 'NONE' , 'NONE' ,  #5114, #1639 ) ;
#1819 = CARTESIAN_POINT ( 'NONE',  ( -14.97509118869195888, 99.49999999999998579, 15.26515554624281101 ) ) ;
#1820 = DIRECTION ( 'NONE',  ( -0.000000000000000000, 1.000000000000000000, -0.000000000000000000 ) ) ;
#1821 = CARTESIAN_POINT ( 'NONE',  ( 19.39806930854667399, 1.749999998907525223, 19.39806930854668465 ) ) ;
#1822 = DIRECTION ( 'NONE',  ( 0.5074415416931677969, 0.000000000000000000, 0.8616861851997287269 ) ) ;
#1823 = EDGE_CURVE ( 'NONE', #8910, #4703, #4211, .T. ) ;
#1824 = CARTESIAN_POINT ( 'NONE',  ( -1.250000000000000222, -1.424999999999999822, -2.165063509461096825 ) ) ;
#1825 = CARTESIAN_POINT ( 'NONE',  ( 0.000000000000000000, 100.0000000000000000, -27.00000000000000355 ) ) ;
#1826 = CARTESIAN_POINT ( 'NONE',  ( -21.30928386698190025, 99.99999999999997158, -11.02857376369709996 ) ) ;
#1827 = ORIENTED_EDGE ( 'NONE', *, *, #9346, .T. ) ;
#1828 = CARTESIAN_POINT ( 'NONE',  ( -22.08823018108446234, 99.99999999999994316, -9.406177930363766038 ) ) ;
#1829 = CARTESIAN_POINT ( 'NONE',  ( 3.024867170474271116, 99.99999999999995737, -24.05477125543085748 ) ) ;
#1830 = CARTESIAN_POINT ( 'NONE',  ( -16.36254897777739004, 99.50000000000001421, 15.39785597259249350 ) ) ;
#1831 = SHAPE_REPRESENTATION_RELATIONSHIP ( 'NONE' , 'NONE' ,  #4065, #1259 ) ;
#1832 = CARTESIAN_POINT ( 'NONE',  ( 8.540544597724410991, 100.0000000000000000, 19.98924338346217766 ) ) ;
#1833 = CARTESIAN_POINT ( 'NONE',  ( 9.583828860305853681, 99.49999999999998579, 20.68614437522342797 ) ) ;
#1834 = PLANE ( 'NONE',  #4779 ) ;
#1835 = ORIENTED_EDGE ( 'NONE', *, *, #8450, .F. ) ;
#1836 = CARTESIAN_POINT ( 'NONE',  ( -2.256430356250000102, -0.2906249993854829183, -1.302750673588580321 ) ) ;
#1837 = ORIENTED_EDGE ( 'NONE', *, *, #10080, .F. ) ;
#1838 = VERTEX_POINT ( 'NONE', #2692 ) ;
#1839 = CARTESIAN_POINT ( 'NONE',  ( 0.000000000000000000, 0.000000000000000000, -27.00000000000000355 ) ) ;
#1840 = CARTESIAN_POINT ( 'NONE',  ( 3.399971579580567393, 99.50000000000000000, -21.57509867787664248 ) ) ;
#1841 = CARTESIAN_POINT ( 'NONE',  ( 3.689266881520847807, 99.50000000000000000, -22.97735580002706968 ) ) ;
#1842 = DIRECTION ( 'NONE',  ( 0.000000000000000000, -1.000000000000000000, 0.000000000000000000 ) ) ;
#1843 = EDGE_CURVE ( 'NONE', #5137, #7619, #7379, .T. ) ;
#1844 = EDGE_CURVE ( 'NONE', #8603, #3561, #8215, .T. ) ;
#1845 = CARTESIAN_POINT ( 'NONE',  ( 8.132491713109025966, 99.50000000000000000, 21.08089001807756091 ) ) ;
#1846 = CARTESIAN_POINT ( 'NONE',  ( 3.306546357697854128E-15, 100.0000000000000000, 27.00000000000000355 ) ) ;
#1847 = LINE ( 'NONE', #8152, #4801 ) ;
#1848 = CARTESIAN_POINT ( 'NONE',  ( -4.357666448243394824E-15, -2.587499999999999467, 2.500000000000000000 ) ) ;
#1849 = CYLINDRICAL_SURFACE ( 'NONE', #893, 18.00000000000000000 ) ;
#1850 = CARTESIAN_POINT ( 'NONE',  ( -27.43301270000000258, 0.7499999989075251117, -3.359575119402369376E-15 ) ) ;
#1851 = CARTESIAN_POINT ( 'NONE',  ( 0.000000000000000000, 97.50000000000000000, -25.00000000000000000 ) ) ;
#1852 = VECTOR ( 'NONE', #5066, 1000.000000000000227 ) ;
#1853 = CARTESIAN_POINT ( 'NONE',  ( 3.097283534322414766, 99.50000000000002842, -24.18405864774921454 ) ) ;
#1854 = CARTESIAN_POINT ( 'NONE',  ( 4.128176300878408256, 99.99999999999998579, -21.47174600747824869 ) ) ;
#1855 = ORIENTED_EDGE ( 'NONE', *, *, #9459, .F. ) ;
#1856 = CARTESIAN_POINT ( 'NONE',  ( 3.373335371007685435, 99.50000000000000000, -22.75111425220066863 ) ) ;
#1857 = CARTESIAN_POINT ( 'NONE',  ( 26.99999999999999645, 5.349999997815049646, 11.18376618407358691 ) ) ;
#1858 = CARTESIAN_POINT ( 'NONE',  ( -20.52076770522338833, 99.50000000000000000, -10.69798695537560462 ) ) ;
#1859 = CARTESIAN_POINT ( 'NONE',  ( -20.97771390646102319, 99.50000000000002842, -10.03345247102482674 ) ) ;
#1860 = CARTESIAN_POINT ( 'NONE',  ( 3.750007936853901658, 100.0000000000000142, -22.95001988029826734 ) ) ;
#1861 = VECTOR ( 'NONE', #6954, 1000.000000000000000 ) ;
#1862 = CARTESIAN_POINT ( 'NONE',  ( 6.246869686064662197, 100.0000000000000000, 20.92172973853146090 ) ) ;
#1863 = CARTESIAN_POINT ( 'NONE',  ( -3.486133158594716510E-16, -0.5062499987709657701, -2.500000000000000000 ) ) ;
#1864 = FACE_OUTER_BOUND ( 'NONE', #9659, .T. ) ;
#1865 = ORIENTED_EDGE ( 'NONE', *, *, #1352, .T. ) ;
#1866 = CARTESIAN_POINT ( 'NONE',  ( 1.249999999999999334, -0.1499999999999999944, -2.165063509461096825 ) ) ;
#1867 =( NAMED_UNIT ( * ) PLANE_ANGLE_UNIT ( ) SI_UNIT ( $, .RADIAN. ) );
#1868 = CARTESIAN_POINT ( 'NONE',  ( -14.97579057656165169, 99.50000000000001421, 16.56690896377573452 ) ) ;
#1869 = DIRECTION ( 'NONE',  ( -0.000000000000000000, 1.000000000000000000, -0.000000000000000000 ) ) ;
#1870 = MECHANICAL_DESIGN_GEOMETRIC_PRESENTATION_REPRESENTATION (  '', ( #9415 ), #8052 ) ;
#1871 = B_SPLINE_CURVE_WITH_KNOTS ( 'NONE', 3,
 ( #3407, #5076, #4299, #5775, #10092, #6602, #8225 ),
 .UNSPECIFIED., .F., .F.,
 ( 4, 1, 1, 1, 4 ),
 ( 0.000000000000000000, 0.2687002788711734813, 0.5225003893189538173, 0.7676814173175746658, 1.000000000000000000 ),
 .UNSPECIFIED. ) ;
#1872 = CARTESIAN_POINT ( 'NONE',  ( 11.36312591709336139, 2.799999998907525267, -27.43301270000000258 ) ) ;
#1873 = CARTESIAN_POINT ( 'NONE',  ( -2.500000000000000000, -0.9375000000000000000, -1.443375672974064106 ) ) ;
#1874 = CARTESIAN_POINT ( 'NONE',  ( 9.342627931057743140, 99.50000000000000000, 21.59831790269294771 ) ) ;
#1875 = DIRECTION ( 'NONE',  ( -0.05422338932609765960, 0.000000000000000000, -0.9985288298541962204 ) ) ;
#1876 = CARTESIAN_POINT ( 'NONE',  ( 8.223467485077383898, 99.99999999999997158, 19.78581333328655134 ) ) ;
#1877 = VERTEX_POINT ( 'NONE', #387 ) ;
#1878 = CARTESIAN_POINT ( 'NONE',  ( -21.49703851962343037, 99.99999999999991473, -9.300281078773625865 ) ) ;
#1879 = CARTESIAN_POINT ( 'NONE',  ( 9.500395184910136237, 99.50000000000000000, 21.12540332933289733 ) ) ;
#1880 = EDGE_CURVE ( 'NONE', #2411, #4835, #5392, .T. ) ;
#1881 = CARTESIAN_POINT ( 'NONE',  ( -2.500000000000000000, -1.743749998770965925, 0.000000000000000000 ) ) ;
#1882 = CARTESIAN_POINT ( 'NONE',  ( 1.250000000000001110, -2.493749998770965703, 2.165063509461096380 ) ) ;
#1883 = CARTESIAN_POINT ( 'NONE',  ( 9.431378708427812896, 99.99999999999992895, 21.34379071326255684 ) ) ;
#1884 = CARTESIAN_POINT ( 'NONE',  ( -21.13452028402337035, 100.0000000000000000, -9.824917503107416294 ) ) ;
#1885 = ORIENTED_EDGE ( 'NONE', *, *, #7543, .T. ) ;
#1886 = CARTESIAN_POINT ( 'NONE',  ( -16.34021191015031249, 100.0000000000000000, 16.45483272884350967 ) ) ;
#1887 = CARTESIAN_POINT ( 'NONE',  ( -2.500000000000000000, -4.031249998770966236, -1.443375672974064106 ) ) ;
#1888 = ORIENTED_EDGE ( 'NONE', *, *, #722, .T. ) ;
#1889 = CARTESIAN_POINT ( 'NONE',  ( -22.31230063665282515, 99.99999999999994316, -10.62159318200525249 ) ) ;
#1890 = DIRECTION ( 'NONE',  ( -0.9567206510497618943, 0.000000000000000000, 0.2910078965507976179 ) ) ;
#1891 = EDGE_CURVE ( 'NONE', #3613, #7437, #3709, .T. ) ;
#1892 = CARTESIAN_POINT ( 'NONE',  ( 4.154273145530666511, 100.0000000000000000, -22.82723029927519676 ) ) ;
#1893 = CARTESIAN_POINT ( 'NONE',  ( -4.959819536546781389E-15, 3.599999997815050534, 27.00000000000000355 ) ) ;
#1894 = CARTESIAN_POINT ( 'NONE',  ( -20.66628160326443364, 99.50000000000001421, -10.01789642611028874 ) ) ;
#1895 =( BOUNDED_CURVE ( )  B_SPLINE_CURVE ( 2, ( #8730, #6369, #1553, #28, #7939, #716, #5690, #773, #4899 ),
 .UNSPECIFIED., .F., .F. ) 
 B_SPLINE_CURVE_WITH_KNOTS ( ( 3, 2, 2, 2, 3 ),
 ( 0.5625000000000000000, 0.5694444444444444198, 0.5833333333333333703, 0.5972222222222222099, 0.6041666666666667407 ),
 .UNSPECIFIED. ) 
 CURVE ( )  GEOMETRIC_REPRESENTATION_ITEM ( )  RATIONAL_B_SPLINE_CURVE ( ( 0.9330127018922194093, 0.9330127018922194093, 1.000000000000000000, 0.8660254037844387076, 1.000000000000000000, 0.8660254037844387076, 1.000000000000000000, 0.9330127018922187432, 0.9330127018922192983 ) ) 
 REPRESENTATION_ITEM ( '' )  );
#1896 = LINE ( 'NONE', #8343, #2492 ) ;
#1897 = EDGE_CURVE ( 'NONE', #4746, #8517, #7219, .T. ) ;
#1898 = LINE ( 'NONE', #1753, #5297 ) ;
#1899 = CARTESIAN_POINT ( 'NONE',  ( 3.664124300404482337, 99.50000000000002842, -24.27219056640880623 ) ) ;
#1900 = VERTEX_POINT ( 'NONE', #1018 ) ;
#1901 = ADVANCED_FACE ( 'NONE', ( #6612 ), #3755, .T. ) ;
#1902 = CYLINDRICAL_SURFACE ( 'NONE', #3076, 2.500000000000000000 ) ;
#1903 = CARTESIAN_POINT ( 'NONE',  ( -27.43301270000000258, 3.149999998907524912, -3.359575119402369376E-15 ) ) ;
#1904 = DIRECTION ( 'NONE',  ( -0.7071067811865477948, 0.000000000000000000, 0.7071067811865473507 ) ) ;
#1905 = CARTESIAN_POINT ( 'NONE',  ( 9.877377282685029372E-16, -4.387499999999999289, 2.500000000000000000 ) ) ;
#1906 = CARTESIAN_POINT ( 'NONE',  ( 8.133363296361027395, 99.50000000000004263, 19.85287606700953233 ) ) ;
#1907 = EDGE_CURVE ( 'NONE', #1313, #10278, #6130, .T. ) ;
#1908 = VERTEX_POINT ( 'NONE', #3803 ) ;
#1909 = CARTESIAN_POINT ( 'NONE',  ( 3.563396934924631942, 99.50000000000001421, -22.47881610735839431 ) ) ;
#1910 = CARTESIAN_POINT ( 'NONE',  ( 1.653273178848927064E-15, 3.999999997815050889, -27.00000000000000355 ) ) ;
#1911 = DIRECTION ( 'NONE',  ( 0.000000000000000000, -1.000000000000000000, 0.000000000000000000 ) ) ;
#1912 = CARTESIAN_POINT ( 'NONE',  ( 1.034219503716432668E-14, -4.556249998770965703, -2.500000000000000000 ) ) ;
#1913 = SURFACE_STYLE_USAGE ( .BOTH. , #7618 ) ;
#1914 = CARTESIAN_POINT ( 'NONE',  ( -21.99951964646687941, 100.0000000000000142, -11.00094659099690553 ) ) ;
#1915 = DIRECTION ( 'NONE',  ( 0.000000000000000000, 0.000000000000000000, -1.000000000000000000 ) ) ;
#1916 = CARTESIAN_POINT ( 'NONE',  ( -2.256430356250000102, -5.090624999385482852, 0.000000000000000000 ) ) ;
#1917 = VECTOR ( 'NONE', #7118, 1000.000000000000000 ) ;
#1918 = EDGE_CURVE ( 'NONE', #1242, #2167, #10129, .T. ) ;
#1919 = CARTESIAN_POINT ( 'NONE',  ( 1.249999999999999334, -2.849999999999999645, -2.165063509461096825 ) ) ;
#1920 = SURFACE_STYLE_USAGE ( .BOTH. , #4236 ) ;
#1921 = DIRECTION ( 'NONE',  ( 0.000000000000000000, 1.000000000000000000, 0.000000000000000000 ) ) ;
#1922 = FACE_OUTER_BOUND ( 'NONE', #6392, .T. ) ;
#1923 = CARTESIAN_POINT ( 'NONE',  ( 27.43301270000000258, 4.249999998907525445, 0.000000000000000000 ) ) ;
#1924 = CARTESIAN_POINT ( 'NONE',  ( -11.18376618407356737, 0.2500000000000000000, -27.00000000000000355 ) ) ;
#1925 = CARTESIAN_POINT ( 'NONE',  ( 3.061616997868383141E-16, 0.000000000000000000, 2.500000000000000000 ) ) ;
#1926 = CARTESIAN_POINT ( 'NONE',  ( 4.311343222282856047, 100.0000000000000000, -24.33387958695581688 ) ) ;
#1927 = CARTESIAN_POINT ( 'NONE',  ( 7.856939908706818798, 100.0000000000000142, 20.19612520319305560 ) ) ;
#1928 = ORIENTED_EDGE ( 'NONE', *, *, #4088, .T. ) ;
#1929 = CARTESIAN_POINT ( 'NONE',  ( -21.89277277937676303, 99.49999999999998579, -9.329958722595300458 ) ) ;
#1930 = CARTESIAN_POINT ( 'NONE',  ( -1.249999999999998224, -5.268749998770966059, 2.165063509461097713 ) ) ;
#1931 = CARTESIAN_POINT ( 'NONE',  ( 3.350143586568126164, 100.0000000000000142, -24.46212657588250394 ) ) ;
#1932 = CARTESIAN_POINT ( 'NONE',  ( 9.513000527211589841, 99.50000000000000000, 20.35102222961602436 ) ) ;
#1933 =( LENGTH_UNIT ( ) NAMED_UNIT ( * ) SI_UNIT ( .MILLI., .METRE. ) );
#1934 = CARTESIAN_POINT ( 'NONE',  ( 0.000000000000000000, 5.000000000000004441, -27.00000000000000355 ) ) ;
#1935 = CARTESIAN_POINT ( 'NONE',  ( 9.500395184910136237, 99.50000000000000000, 21.12540332933289733 ) ) ;
#1936 = AXIS2_PLACEMENT_3D ( 'NONE', #4316, #1681, #9133 ) ;
#1937 = DIRECTION ( 'NONE',  ( -0.000000000000000000, 1.000000000000000000, -0.000000000000000000 ) ) ;
#1938 = EDGE_LOOP ( 'NONE', ( #1426, #6837, #5410, #6885 ) ) ;
#1939 = CARTESIAN_POINT ( 'NONE',  ( 8.132491713109025966, 99.50000000000000000, 21.08089001807756091 ) ) ;
#1940 = AXIS2_PLACEMENT_3D ( 'NONE', #5406, #3725, #2205 ) ;
#1941 = CARTESIAN_POINT ( 'NONE',  ( -2.256430356249999214, -1.115624999385482763, 1.302750673588581876 ) ) ;
#1942 = ORIENTED_EDGE ( 'NONE', *, *, #6701, .T. ) ;
#1943 = CARTESIAN_POINT ( 'NONE',  ( -22.43115009631934953, 99.50000000000001421, -11.08196351649073819 ) ) ;
#1944 = DIRECTION ( 'NONE',  ( -0.000000000000000000, 1.000000000000000000, -0.000000000000000000 ) ) ;
#1945 = CARTESIAN_POINT ( 'NONE',  ( 3.374624233514611937, 99.50000000000002842, -23.25900349070959550 ) ) ;
#1946 = CARTESIAN_POINT ( 'NONE',  ( 4.599186066243659887, 100.0000000000000568, -24.59301055568561623 ) ) ;
#1947 = STYLED_ITEM ( 'NONE', ( #7417 ), #5870 ) ;
#1948 = ORIENTED_EDGE ( 'NONE', *, *, #5357, .T. ) ;
#1949 = EDGE_CURVE ( 'NONE', #6063, #9655, #8128, .T. ) ;
#1950 = CARTESIAN_POINT ( 'NONE',  ( -15.15623813234777018, 99.50000000000000000, 16.19783826294960249 ) ) ;
#1951 = CARTESIAN_POINT ( 'NONE',  ( -1.249999999999998224, -0.7687499987709658367, 2.165063509461097713 ) ) ;
#1952 = DIRECTION ( 'NONE',  ( 6.123233995736763571E-17, 0.000000000000000000, -1.000000000000000000 ) ) ;
#1953 = CARTESIAN_POINT ( 'NONE',  ( 9.861577898019769250, 99.99999999999995737, 21.03794551367759169 ) ) ;
#1954 = ORIENTED_EDGE ( 'NONE', *, *, #1891, .T. ) ;
#1955 = DIRECTION ( 'NONE',  ( -0.2149789550291109352, 0.000000000000000000, -0.9766186814179788067 ) ) ;
#1956 = CARTESIAN_POINT ( 'NONE',  ( 27.43301270000000258, 5.199999998907525622, -11.36312591709336139 ) ) ;
#1957 = DIRECTION ( 'NONE',  ( -0.000000000000000000, -1.000000000000000000, 0.000000000000000000 ) ) ;
#1958 = CARTESIAN_POINT ( 'NONE',  ( 3.606694021351891877, 99.50000000000000000, -24.61315535935035115 ) ) ;
#1959 = CARTESIAN_POINT ( 'NONE',  ( 7.978247738654171251, 99.99999999999994316, 20.00924965157036794 ) ) ;
#1960 = CARTESIAN_POINT ( 'NONE',  ( 9.802580223201115217, 99.49999999999997158, 21.25247094773282086 ) ) ;
#1961 = CARTESIAN_POINT ( 'NONE',  ( 1.653273178848927064E-15, 2.399999997815050357, -27.00000000000000355 ) ) ;
#1962 =( BOUNDED_CURVE ( )  B_SPLINE_CURVE ( 2, ( #6014, #10045, #2883, #3049, #7855, #581, #5459, #6961, #6066 ),
 .UNSPECIFIED., .F., .F. ) 
 B_SPLINE_CURVE_WITH_KNOTS ( ( 3, 2, 2, 2, 3 ),
 ( 0.4791666666666666852, 0.4861111111111111049, 0.5000000000000000000, 0.5138888888888888395, 0.5208333333333333703 ),
 .UNSPECIFIED. ) 
 CURVE ( )  GEOMETRIC_REPRESENTATION_ITEM ( )  RATIONAL_B_SPLINE_CURVE ( ( 0.9330127018922194093, 0.9330127018922196314, 1.000000000000000000, 0.8660254037844387076, 1.000000000000000000, 0.8660254037844387076, 1.000000000000000000, 0.9330127018922187432, 0.9330127018922192983 ) ) 
 REPRESENTATION_ITEM ( '' )  );
#1963 =( NAMED_UNIT ( * ) PLANE_ANGLE_UNIT ( ) SI_UNIT ( $, .RADIAN. ) );
#1964 = CARTESIAN_POINT ( 'NONE',  ( 0.000000000000000000, 85.00000000000000000, 0.000000000000000000 ) ) ;
#1965 = ORIENTED_EDGE ( 'NONE', *, *, #227, .T. ) ;
#1966 = CARTESIAN_POINT ( 'NONE',  ( 4.852629679480013891, 99.50000000000001421, -23.84752007312514621 ) ) ;
#1967 = CARTESIAN_POINT ( 'NONE',  ( -2.500000000000000000, 0.000000000000000000, 0.000000000000000000 ) ) ;
#1968 = VERTEX_POINT ( 'NONE', #4468 ) ;
#1969 = CARTESIAN_POINT ( 'NONE',  ( 5.302876193624534821E-16, -1.237499999999999822, 2.886751345948128655 ) ) ;
#1970 = APPLICATION_PROTOCOL_DEFINITION ( 'draft international standard', 'automotive_design', 1998, #2467 ) ;
#1971 = CARTESIAN_POINT ( 'NONE',  ( -1.250000000000000222, -2.774999999999999467, -2.165063509461096825 ) ) ;
#1972 = FACE_OUTER_BOUND ( 'NONE', #7310, .T. ) ;
#1973 = EDGE_CURVE ( 'NONE', #10278, #5989, #2527, .T. ) ;
#1974 = CARTESIAN_POINT ( 'NONE',  ( -27.43301270000000258, 1.399999998907525134, -11.36312591709336317 ) ) ;
#1975 = CARTESIAN_POINT ( 'NONE',  ( -27.00000000000001421, 0.4500000000000000666, 11.18376618407356560 ) ) ;
#1976 = VERTEX_POINT ( 'NONE', #2173 ) ;
#1977 = EDGE_CURVE ( 'NONE', #6767, #872, #6929, .T. ) ;
#1978 = CARTESIAN_POINT ( 'NONE',  ( -1.249999999999998224, -1.274999999999999911, 2.165063509461097713 ) ) ;
#1979 = CARTESIAN_POINT ( 'NONE',  ( 0.000000000000000000, 0.000000000000000000, 0.000000000000000000 ) ) ;
#1980 = DIRECTION ( 'NONE',  ( -0.000000000000000000, -0.000000000000000000, -1.000000000000000000 ) ) ;
#1981 = CARTESIAN_POINT ( 'NONE',  ( 7.783718120363267268, 99.49999999999998579, 21.09473326129887027 ) ) ;
#1982 = DIRECTION ( 'NONE',  ( 0.000000000000000000, 0.000000000000000000, -1.000000000000000000 ) ) ;
#1983 = ORIENTED_EDGE ( 'NONE', *, *, #172, .F. ) ;
#1984 = FACE_OUTER_BOUND ( 'NONE', #10327, .T. ) ;
#1985 = CARTESIAN_POINT ( 'NONE',  ( 9.389534246205572643, 99.50000000000001421, 21.46805835725047729 ) ) ;
#1986 = CARTESIAN_POINT ( 'NONE',  ( -16.56926954694585774, 99.99999999999997158, 15.12296757606276643 ) ) ;
#1987 = CARTESIAN_POINT ( 'NONE',  ( 9.547662139763570366, 99.49999999999997158, 20.94662037603165672 ) ) ;
#1988 = CARTESIAN_POINT ( 'NONE',  ( 27.00000000000000355, 2.449999999999999734, -11.18376618407356915 ) ) ;
#1989 = EDGE_LOOP ( 'NONE', ( #6193, #2273, #7966, #5164 ) ) ;
#1990 = CARTESIAN_POINT ( 'NONE',  ( -16.35834224700816009, 100.0000000000000000, 16.43761959438736397 ) ) ;
#1991 = CARTESIAN_POINT ( 'NONE',  ( 1.128215178124999607, -2.203124999385482674, -1.954126010382871259 ) ) ;
#1992 = VERTEX_POINT ( 'NONE', #3850 ) ;
#1993 = CARTESIAN_POINT ( 'NONE',  ( 4.739008722453744049, 99.50000000000001421, -24.06821587619827696 ) ) ;
#1994 = CARTESIAN_POINT ( 'NONE',  ( 2.500000000000000000, -0.6749999999999999334, -3.061616997868383141E-16 ) ) ;
#1995 = CARTESIAN_POINT ( 'NONE',  ( -7.500000000000000000, 104.5000000000000142, -0.9999999999999997780 ) ) ;
#1996 = CARTESIAN_POINT ( 'NONE',  ( -15.22320097062094568, 100.0000000000000142, 16.32303119091969634 ) ) ;
#1997 = EDGE_LOOP ( 'NONE', ( #7091, #7609, #5760, #4747 ) ) ;
#1998 = CARTESIAN_POINT ( 'NONE',  ( -1.250000000000000222, -0.4687499987709658478, -2.165063509461096825 ) ) ;
#1999 = CARTESIAN_POINT ( 'NONE',  ( -16.84090648038580085, 99.99999999999998579, 15.49469789757679727 ) ) ;
#2000 = CARTESIAN_POINT ( 'NONE',  ( 3.535161742238301041, 99.50000000000001421, -24.18247714022527006 ) ) ;
#2001 = ORIENTED_EDGE ( 'NONE', *, *, #184, .F. ) ;
#2002 = FACE_OUTER_BOUND ( 'NONE', #3692, .T. ) ;
#2003 = CARTESIAN_POINT ( 'NONE',  ( 27.43301269999999548, 2.699999998907525178, 11.36312591709337738 ) ) ;
#2004 = DIRECTION ( 'NONE',  ( -1.000000000000000000, 0.000000000000000000, 0.000000000000000000 ) ) ;
#2005 = EDGE_CURVE ( 'NONE', #3644, #8551, #5372, .T. ) ;
#2006 = CARTESIAN_POINT ( 'NONE',  ( -16.70213339477928471, 99.99999999999998579, 16.52464093453885852 ) ) ;
#2007 = EDGE_LOOP ( 'NONE', ( #8523, #10020, #4656, #6965 ) ) ;
#2008 = CARTESIAN_POINT ( 'NONE',  ( -21.89277277937676303, 99.99999999999998579, -9.329958722595300458 ) ) ;
#2009 = FACE_OUTER_BOUND ( 'NONE', #9388, .T. ) ;
#2010 = LINE ( 'NONE', #6781, #10027 ) ;
#2011 = DIRECTION ( 'NONE',  ( -0.000000000000000000, -0.000000000000000000, -1.000000000000000000 ) ) ;
#2012 = CARTESIAN_POINT ( 'NONE',  ( 3.689266881520847807, 100.0000000000000000, -22.97735580002706968 ) ) ;
#2013 = VERTEX_POINT ( 'NONE', #3272 ) ;
#2014 = B_SPLINE_CURVE_WITH_KNOTS ( 'NONE', 3,
 ( #8567, #1393, #608, #6990, #5435, #8625, #1447 ),
 .UNSPECIFIED., .F., .F.,
 ( 4, 1, 1, 1, 4 ),
 ( 0.000000000000000000, 0.2581490702850675056, 0.5078756004687992043, 0.7540928115589713432, 1.000000000000000000 ),
 .UNSPECIFIED. ) ;
#2015 = CARTESIAN_POINT ( 'NONE',  ( -15.98972951825121669, 99.99999999999997158, 15.19400804711857411 ) ) ;
#2016 = CIRCLE ( 'NONE', #6212, 22.50000000000000355 ) ;
#2017 = CARTESIAN_POINT ( 'NONE',  ( 11.36312591709336850, 2.599999998907525534, 27.43301269999999903 ) ) ;
#2018 = AXIS2_PLACEMENT_3D ( 'NONE', #3168, #119, #3215 ) ;
#2019 = ORIENTED_EDGE ( 'NONE', *, *, #4043, .T. ) ;
#2020 = CARTESIAN_POINT ( 'NONE',  ( -1.249999999999998224, -2.174999999999999822, 2.165063509461097713 ) ) ;
#2021 = EDGE_CURVE ( 'NONE', #3170, #3531, #7292, .T. ) ;
#2022 = APPLICATION_PROTOCOL_DEFINITION ( 'draft international standard', 'automotive_design', 1998, #7453 ) ;
#2023 = LINE ( 'NONE', #9990, #1257 ) ;
#2024 =( BOUNDED_CURVE ( )  B_SPLINE_CURVE ( 2, ( #3510, #5182, #2839, #5867, #1881, #7533, #3462, #1159, #2677 ),
 .UNSPECIFIED., .F., .T. ) 
 B_SPLINE_CURVE_WITH_KNOTS ( ( 3, 2, 2, 2, 3 ),
 ( 0.2291666666666666574, 0.2361111111111111049, 0.2500000000000000000, 0.2638888888888888951, 0.2708333333333333703 ),
 .UNSPECIFIED. ) 
 CURVE ( )  GEOMETRIC_REPRESENTATION_ITEM ( )  RATIONAL_B_SPLINE_CURVE ( ( 0.9330127018922194093, 0.9330127018922194093, 1.000000000000000000, 0.8660254037844387076, 1.000000000000000000, 0.8660254037844387076, 1.000000000000000000, 0.9330127018922190762, 0.9330127018922194093 ) ) 
 REPRESENTATION_ITEM ( '' )  );
#2025 = CARTESIAN_POINT ( 'NONE',  ( 2.256430356250000546, -2.315624999385482496, 1.302750673588579877 ) ) ;
#2026 = CARTESIAN_POINT ( 'NONE',  ( -5.039362679103552881E-15, 4.049999998907525267, 27.43301270000000258 ) ) ;
#2027 = CARTESIAN_POINT ( 'NONE',  ( -7.500000000000000000, 104.5000000000000142, 1.000000000000000222 ) ) ;
#2028 = VERTEX_POINT ( 'NONE', #79 ) ;
#2029 = AXIS2_PLACEMENT_3D ( 'NONE', #10176, #10116, #6975 ) ;
#2030 = CARTESIAN_POINT ( 'NONE',  ( -15.29853103387017121, 100.0000000000000142, 14.98378122532347057 ) ) ;
#2031 = EDGE_CURVE ( 'NONE', #2682, #8581, #963, .T. ) ;
#2032 = DIRECTION ( 'NONE',  ( 0.000000000000000000, 1.430867686834485556E-12, -1.000000000000000000 ) ) ;
#2033 = CARTESIAN_POINT ( 'NONE',  ( -16.30857500771091040, 99.99999999999994316, 15.34700649443169063 ) ) ;
#2034 = CARTESIAN_POINT ( 'NONE',  ( 2.256430356250000546, -1.753124999385482496, 1.302750673588579877 ) ) ;
#2035 = CARTESIAN_POINT ( 'NONE',  ( -2.500000000000000000, -5.343749998770965348, 0.000000000000000000 ) ) ;
#2036 = ORIENTED_EDGE ( 'NONE', *, *, #5758, .F. ) ;
#2037 = EDGE_CURVE ( 'NONE', #7672, #7769, #9181, .T. ) ;
#2038 = CARTESIAN_POINT ( 'NONE',  ( -2.256430356250000102, -0.1406249993854829516, 0.000000000000000000 ) ) ;
#2039 = CARTESIAN_POINT ( 'NONE',  ( -19.39806930854667755, 1.349999998907525312, -19.39806930854668110 ) ) ;
#2040 = AXIS2_PLACEMENT_3D ( 'NONE', #2702, #1957, #2004 ) ;
#2041 = EDGE_CURVE ( 'NONE', #486, #7555, #365, .T. ) ;
#2042 = PRESENTATION_STYLE_ASSIGNMENT (( #5414 ) ) ;
#2043 = CARTESIAN_POINT ( 'NONE',  ( 11.18376618407357093, 4.950000000000000178, -27.00000000000000355 ) ) ;
#2044 = DIRECTION ( 'NONE',  ( -0.000000000000000000, 1.000000000000000000, -0.000000000000000000 ) ) ;
#2045 = FACE_OUTER_BOUND ( 'NONE', #5499, .T. ) ;
#2046 = ORIENTED_EDGE ( 'NONE', *, *, #5317, .T. ) ;
#2047 = ORIENTED_EDGE ( 'NONE', *, *, #7593, .F. ) ;
#2048 = DIRECTION ( 'NONE',  ( -0.000000000000000000, -1.000000000000000000, -0.000000000000000000 ) ) ;
#2049 = MECHANICAL_DESIGN_GEOMETRIC_PRESENTATION_REPRESENTATION (  '', ( #2563 ), #9589 ) ;
#2050 = CARTESIAN_POINT ( 'NONE',  ( 2.256430356249999658, -0.8906249993854827851, -1.302750673588581432 ) ) ;
#2051 = ORIENTED_EDGE ( 'NONE', *, *, #42, .F. ) ;
#2052 = CARTESIAN_POINT ( 'NONE',  ( 4.311343222282856047, 99.50000000000000000, -24.33387958695581688 ) ) ;
#2053 = CARTESIAN_POINT ( 'NONE',  ( 0.6698729810778075722, -0.7674038105676657118, 2.499999999999999556 ) ) ;
#2054 = CARTESIAN_POINT ( 'NONE',  ( 2.500000000000000000, -0.1874999999999999722, -1.443375672974065438 ) ) ;
#2055 = CARTESIAN_POINT ( 'NONE',  ( -19.09188309203678813, 5.099999997815051422, 19.09188309203678457 ) ) ;
#2056 = CARTESIAN_POINT ( 'NONE',  ( 5.179363668139080445, 99.50000000000007105, -23.94265746362379943 ) ) ;
#2057 = MECHANICAL_DESIGN_GEOMETRIC_PRESENTATION_REPRESENTATION (  '', ( #9429 ), #1570 ) ;
#2058 = ORIENTED_EDGE ( 'NONE', *, *, #1465, .T. ) ;
#2059 = CARTESIAN_POINT ( 'NONE',  ( -1.250000000000000222, -0.9187499987709658589, -2.165063509461096825 ) ) ;
#2060 = CARTESIAN_POINT ( 'NONE',  ( -16.90147242988460263, 99.99999999999998579, 15.68472263728856753 ) ) ;
#2061 = CARTESIAN_POINT ( 'NONE',  ( 2.500000000000000000, -2.924999999999999822, -3.061616997868383141E-16 ) ) ;
#2062 = ORIENTED_EDGE ( 'NONE', *, *, #3389, .F. ) ;
#2063 = CARTESIAN_POINT ( 'NONE',  ( 27.00000000000000355, 1.399999997815050579, 0.000000000000000000 ) ) ;
#2064 = CARTESIAN_POINT ( 'NONE',  ( 19.39806930854667399, 5.049999998907525267, 19.39806930854668465 ) ) ;
#2065 = CARTESIAN_POINT ( 'NONE',  ( -0.6698729810778105698, -4.857596189432333844, 2.499999999999997780 ) ) ;
#2066 = CARTESIAN_POINT ( 'NONE',  ( 9.692323321704657602, 99.50000000000001421, 21.58969587442354410 ) ) ;
#2067 = PRODUCT_DEFINITION_SHAPE ( 'NONE', 'NONE',  #10372 ) ;
#2068 = ORIENTED_EDGE ( 'NONE', *, *, #8907, .F. ) ;
#2069 = DIRECTION ( 'NONE',  ( 0.000000000000000000, 0.000000000000000000, -1.000000000000000000 ) ) ;
#2070 = CARTESIAN_POINT ( 'NONE',  ( 8.465276868207817884, 99.50000000000001421, 19.66343818277063704 ) ) ;
#2071 = CARTESIAN_POINT ( 'NONE',  ( 6.477538756577482459, 100.0000000000000000, 20.49684993083915430 ) ) ;
#2072 = CARTESIAN_POINT ( 'NONE',  ( -16.56313167360273297, 99.50000000000002842, 16.06491815633068398 ) ) ;
#2073 = CARTESIAN_POINT ( 'NONE',  ( -1.915120254295647362, -5.000523192925935945, -1.606958123781256464 ) ) ;
#2074 = EDGE_CURVE ( 'NONE', #1371, #2426, #8723, .T. ) ;
#2075 = ORIENTED_EDGE ( 'NONE', *, *, #5985, .T. ) ;
#2076 = CARTESIAN_POINT ( 'NONE',  ( -15.56095293356939813, 100.0000000000000142, 15.23332223661997453 ) ) ;
#2077 = CARTESIAN_POINT ( 'NONE',  ( 27.43301270000000258, 2.799999998907524823, -11.36312591709336139 ) ) ;
#2078 = ORIENTED_EDGE ( 'NONE', *, *, #1453, .T. ) ;
#2079 = CARTESIAN_POINT ( 'NONE',  ( -2.500000000000000000, -2.287499999999999645, -1.443375672974064106 ) ) ;
#2080 = AXIS2_PLACEMENT_3D ( 'NONE', #9368, #8475, #2252 ) ;
#2081 = DIRECTION ( 'NONE',  ( 0.000000000000000000, 0.000000000000000000, 1.000000000000000000 ) ) ;
#2082 = PLANE ( 'NONE',  #2080 ) ;
#2083 = CARTESIAN_POINT ( 'NONE',  ( 2.256430356249999658, -1.790624999385482807, -1.302750673588581432 ) ) ;
#2084 = CARTESIAN_POINT ( 'NONE',  ( 27.43301269999999548, 4.999999998907525445, 11.36312591709337738 ) ) ;
#2085 = CARTESIAN_POINT ( 'NONE',  ( 11.36312591709336850, 2.599999998907525534, 27.43301269999999903 ) ) ;
#2086 = EDGE_LOOP ( 'NONE', ( #4473, #9500, #7186 ) ) ;
#2087 = CARTESIAN_POINT ( 'NONE',  ( -15.70584307919286893, 100.0000000000000000, 14.84247401567675162 ) ) ;
#2088 = CARTESIAN_POINT ( 'NONE',  ( 10.72103337977569204, 100.0000000000000000, 22.20268488987243316 ) ) ;
#2089 = CARTESIAN_POINT ( 'NONE',  ( 7.734522023158566739, 100.0000000000000284, 20.86022014488863618 ) ) ;
#2090 = AXIS2_PLACEMENT_3D ( 'NONE', #7524, #1097, #5813 ) ;
#2091 = ADVANCED_FACE ( 'NONE', ( #5581 ), #4840, .T. ) ;
#2092 = CARTESIAN_POINT ( 'NONE',  ( 1.653273178848927064E-15, 0.7999999978150503788, -27.00000000000000355 ) ) ;
#2093 = EDGE_LOOP ( 'NONE', ( #9850, #7032, #5344, #7027, #3006, #9140 ) ) ;
#2094 = CARTESIAN_POINT ( 'NONE',  ( 1.128215178125001161, -0.8906249993854828961, 1.954126010382870815 ) ) ;
#2095 = CARTESIAN_POINT ( 'NONE',  ( 2.874264611687397331, 100.0000000000000142, -22.24889838548798693 ) ) ;
#2096 = ORIENTED_EDGE ( 'NONE', *, *, #294, .T. ) ;
#2097 = DIRECTION ( 'NONE',  ( -0.000000000000000000, -1.000000000000000000, -0.000000000000000000 ) ) ;
#2098 =( BOUNDED_CURVE ( )  B_SPLINE_CURVE ( 2, ( #1181, #293, #9814, #2650, #1233, #4371, #3485, #4426, #5840 ),
 .UNSPECIFIED., .F., .T. ) 
 B_SPLINE_CURVE_WITH_KNOTS ( ( 3, 2, 2, 2, 3 ),
 ( 0.3125000000000000000, 0.3194444444444444198, 0.3333333333333333148, 0.3472222222222222099, 0.3541666666666666852 ),
 .UNSPECIFIED. ) 
 CURVE ( )  GEOMETRIC_REPRESENTATION_ITEM ( )  RATIONAL_B_SPLINE_CURVE ( ( 0.9330127018922194093, 0.9330127018922194093, 1.000000000000000000, 0.8660254037844387076, 1.000000000000000000, 0.8660254037844387076, 1.000000000000000000, 0.9330127018922190762, 0.9330127018922194093 ) ) 
 REPRESENTATION_ITEM ( '' )  );
#2099 = CARTESIAN_POINT ( 'NONE',  ( 27.43301269999999548, 2.599999998907525089, 11.36312591709337738 ) ) ;
#2100 = PRESENTATION_STYLE_ASSIGNMENT (( #9266 ) ) ;
#2101 = DIRECTION ( 'NONE',  ( -0.000000000000000000, 1.000000000000000000, -0.000000000000000000 ) ) ;
#2102 = CARTESIAN_POINT ( 'NONE',  ( 1.653273178848927064E-15, 1.000000000000000000, -27.00000000000000355 ) ) ;
#2103 = CARTESIAN_POINT ( 'NONE',  ( 8.757234875838378230, 100.0000000000000284, 19.92790116963689329 ) ) ;
#2104 = VERTEX_POINT ( 'NONE', #2538 ) ;
#2105 = LINE ( 'NONE', #1939, #6229 ) ;
#2106 = CARTESIAN_POINT ( 'NONE',  ( 4.786228327491941173E-16, -2.840624999385482852, 2.605501347177161087 ) ) ;
#2107 = VERTEX_POINT ( 'NONE', #1739 ) ;
#2108 = CARTESIAN_POINT ( 'NONE',  ( 4.584380863705032283, 99.50000000000001421, -24.21384527865288305 ) ) ;
#2109 = DIRECTION ( 'NONE',  ( 0.000000000000000000, 1.000000000000000000, 0.000000000000000000 ) ) ;
#2110 = CARTESIAN_POINT ( 'NONE',  ( 9.877377282685029372E-16, -0.3374999999999999667, 2.500000000000000000 ) ) ;
#2111 = AXIS2_PLACEMENT_3D ( 'NONE', #9162, #4559, #1982 ) ;
#2112 = CARTESIAN_POINT ( 'NONE',  ( 1.128215178125001161, -0.5531249993854828739, 1.954126010382870815 ) ) ;
#2113 = CARTESIAN_POINT ( 'NONE',  ( 5.240996349771887886, 100.0000000000000426, -23.60769396873743631 ) ) ;
#2114 = B_SPLINE_CURVE_WITH_KNOTS ( 'NONE', 3,
 ( #8736, #6328, #3090, #8047, #673, #1560, #831, #2400, #4751, #779, #881, #3973, #7158, #5595, #3866, #5647, #7254, #9619, #4072 ),
 .UNSPECIFIED., .F., .F.,
 ( 4, 1, 1, 1, 1, 1, 1, 1, 1, 1, 1, 1, 1, 1, 1, 1, 4 ),
 ( 0.000000000000000000, 0.06441145199513656494, 0.1272798026707614161, 0.1891796676955485867, 0.2501048626594916668, 0.3106574229659737063, 0.3727353219478334867, 0.4357106927796215445, 0.5001540812204312569, 0.5646670943021733224, 0.6273118991093056263, 0.6892359343283066542, 0.7500873997029591234, 0.8110709007071082999, 0.8723115105649058565, 0.9354174373376444862, 1.000000000000000000 ),
 .UNSPECIFIED. ) ;
#2115 = CIRCLE ( 'NONE', #3631, 7.500000000000000000 ) ;
#2116 = ADVANCED_FACE ( 'NONE', ( #3957 ), #22, .F. ) ;
#2117 = AXIS2_PLACEMENT_3D ( 'NONE', #2132, #2192, #6052 ) ;
#2118 = CARTESIAN_POINT ( 'NONE',  ( 3.681717055787076642, 99.50000000000000000, -21.09125273517263111 ) ) ;
#2119 = CARTESIAN_POINT ( 'NONE',  ( -4.959819536546781389E-15, 1.399999999999999911, 27.00000000000000355 ) ) ;
#2120 = DIRECTION ( 'NONE',  ( 0.000000000000000000, -1.000000000000000000, 0.000000000000000000 ) ) ;
#2121 = ORIENTED_EDGE ( 'NONE', *, *, #1522, .T. ) ;
#2122 = CARTESIAN_POINT ( 'NONE',  ( -17.94007301623892658, 99.50000000000000000, 17.49000340848992607 ) ) ;
#2123 = CARTESIAN_POINT ( 'NONE',  ( -19.39806930854668465, 4.049999998907525267, 19.39806930854667755 ) ) ;
#2124 = CARTESIAN_POINT ( 'NONE',  ( -1.595409442497313560E-16, -0.7031249993854828961, -2.605501347177161087 ) ) ;
#2125 = CARTESIAN_POINT ( 'NONE',  ( 9.873655262861264603, 99.50000000000000000, 20.34710108723753308 ) ) ;
#2126 = CARTESIAN_POINT ( 'NONE',  ( -15.15871127190382417, 99.50000000000000000, 15.63231653451427761 ) ) ;
#2127 = CARTESIAN_POINT ( 'NONE',  ( 0.000000000000000000, -25.00000000000000000, 0.000000000000000000 ) ) ;
#2128 = CARTESIAN_POINT ( 'NONE',  ( 5.226890989224467710, 99.50000000000000000, -23.72545275563321354 ) ) ;
#2129 = CARTESIAN_POINT ( 'NONE',  ( 1.653273178848927064E-15, 3.400000000000000355, -27.00000000000000355 ) ) ;
#2130 = FACE_BOUND ( 'NONE', #2901, .T. ) ;
#2131 = VERTEX_POINT ( 'NONE', #2333 ) ;
#2132 = CARTESIAN_POINT ( 'NONE',  ( 0.000000000000000000, 87.00000000000001421, 0.000000000000000000 ) ) ;
#2133 = CARTESIAN_POINT ( 'NONE',  ( 11.36312591709336139, 0.4999999989075251672, -27.43301270000000258 ) ) ;
#2134 = ORIENTED_EDGE ( 'NONE', *, *, #2246, .T. ) ;
#2135 = VECTOR ( 'NONE', #10163, 1000.000000000000227 ) ;
#2136 = CARTESIAN_POINT ( 'NONE',  ( 2.500000000000000000, -1.125000000000000000, -3.061616997868383141E-16 ) ) ;
#2137 = PRODUCT_CONTEXT ( 'NONE', #5679, 'mechanical' ) ;
#2138 = CARTESIAN_POINT ( 'NONE',  ( -22.51767453479306980, 99.50000000000000000, -9.764155749770198511 ) ) ;
#2139 = CARTESIAN_POINT ( 'NONE',  ( 2.901827748664965068, 99.99999999999995737, -21.68759887446373469 ) ) ;
#2140 = CARTESIAN_POINT ( 'NONE',  ( 2.256430356250000546, -2.765624999385483118, 1.302750673588579877 ) ) ;
#2141 = CARTESIAN_POINT ( 'NONE',  ( -16.79604063091391097, 99.50000000000000000, 15.40463673182947701 ) ) ;
#2142 = CARTESIAN_POINT ( 'NONE',  ( -11.36312591709337383, 1.699999998907525178, 27.43301269999999548 ) ) ;
#2144 = ORIENTED_EDGE ( 'NONE', *, *, #3187, .F. ) ;
#2143 = ORIENTED_EDGE ( 'NONE', *, *, #2423, .T. ) ;
#2145 = UNCERTAINTY_MEASURE_WITH_UNIT (LENGTH_MEASURE( 1.000000000000000082E-05 ), #2268, 'distance_accuracy_value', 'NONE');
#2146 = CARTESIAN_POINT ( 'NONE',  ( 2.500000000000000000, -2.024999999999999911, -3.061616997868383141E-16 ) ) ;
#2147 = VECTOR ( 'NONE', #8884, 1000.000000000000000 ) ;
#2148 = DIRECTION ( 'NONE',  ( 0.000000000000000000, -0.000000000000000000, -1.000000000000000000 ) ) ;
#2149 = CARTESIAN_POINT ( 'NONE',  ( -10.49999999999999822, 104.5000000000000142, 0.000000000000000000 ) ) ;
#2150 = LINE ( 'NONE', #7636, #2463 ) ;
#2151 = ORIENTED_EDGE ( 'NONE', *, *, #2573, .F. ) ;
#2152 = CARTESIAN_POINT ( 'NONE',  ( 2.256430356249999658, -0.7781249993854830738, -1.302750673588581432 ) ) ;
#2153 = CARTESIAN_POINT ( 'NONE',  ( -21.43094455402013310, 99.50000000000000000, -11.42705968398779426 ) ) ;
#2154 = DIRECTION ( 'NONE',  ( 0.4980973490458726061, -0.08715574274765837404, 0.8627299156628209786 ) ) ;
#2155 = CARTESIAN_POINT ( 'NONE',  ( -19.39806930854667755, 3.749999998907525445, -19.39806930854668110 ) ) ;
#2156 = ORIENTED_EDGE ( 'NONE', *, *, #3716, .F. ) ;
#2157 = CARTESIAN_POINT ( 'NONE',  ( 1.250000000000001110, -2.943749998770965437, 2.165063509461096380 ) ) ;
#2158 = EDGE_CURVE ( 'NONE', #3256, #2131, #3898, .T. ) ;
#2159 = CARTESIAN_POINT ( 'NONE',  ( 27.00000000000000355, 0.8500000000000001998, -11.18376618407356737 ) ) ;
#2160 = CARTESIAN_POINT ( 'NONE',  ( 9.446088657802272692, 99.50000000000004263, 20.22669104216016578 ) ) ;
#2161 = EDGE_LOOP ( 'NONE', ( #1509, #3667, #482, #1885, #5735 ) ) ;
#2162 = CARTESIAN_POINT ( 'NONE',  ( 8.540544597724410991, 99.50000000000000000, 19.98924338346217766 ) ) ;
#2163 = CARTESIAN_POINT ( 'NONE',  ( 8.102924533678123709, 100.0000000000000000, 20.98904009517733726 ) ) ;
#2164 = ORIENTED_EDGE ( 'NONE', *, *, #6418, .T. ) ;
#2165 = CARTESIAN_POINT ( 'NONE',  ( -1.128215178125000273, -0.7781249993854828517, -1.954126010382871259 ) ) ;
#2166 = ORIENTED_EDGE ( 'NONE', *, *, #7977, .F. ) ;
#2167 = VERTEX_POINT ( 'NONE', #1543 ) ;
#2168 = B_SPLINE_CURVE_WITH_KNOTS ( 'NONE', 3,
 ( #3512, #429, #9214, #7535, #7432, #9845, #2679, #3627, #5869, #325, #2733, #2784, #6807, #10005, #9385 ),
 .UNSPECIFIED., .F., .F.,
 ( 4, 1, 1, 1, 1, 1, 1, 1, 1, 1, 1, 1, 4 ),
 ( 0.000000000000000000, 0.1055296353700490852, 0.2070742529895955586, 0.3056622059958778448, 0.4023599870273183998, 0.4943057198019382148, 0.5778637904027289496, 0.6550095244395398586, 0.7278863574113029200, 0.7976678238154090161, 0.8645871040366396310, 0.9319858836656568224, 1.000000000000000000 ),
 .UNSPECIFIED. ) ;
#2169 = CARTESIAN_POINT ( 'NONE',  ( -22.55793349878803156, 99.50000000000000000, -10.88926985104519929 ) ) ;
#2170 = CARTESIAN_POINT ( 'NONE',  ( -11.36312591709337561, 0.7999999989075252671, 27.43301269999999548 ) ) ;
#2171 = CARTESIAN_POINT ( 'NONE',  ( -21.04016555629948826, 99.50000000000001421, -9.929603401003973318 ) ) ;
#2172 = CARTESIAN_POINT ( 'NONE',  ( 2.256430356250000546, -2.315624999385482496, 1.302750673588579877 ) ) ;
#2173 = CARTESIAN_POINT ( 'NONE',  ( -24.00000000000000711, 71.18660744634364335, 0.000000000000000000 ) ) ;
#2174 = EDGE_CURVE ( 'NONE', #2880, #4986, #4009, .T. ) ;
#2175 = CARTESIAN_POINT ( 'NONE',  ( 21.79306891025641235, 99.50000000000000000, -1.065004006410256387 ) ) ;
#2176 = CARTESIAN_POINT ( 'NONE',  ( 4.793167276645844410, 99.49999999999998579, -21.69837440717521204 ) ) ;
#2177 = CARTESIAN_POINT ( 'NONE',  ( 1.653273178848927064E-15, 1.000000000000000000, -27.00000000000000355 ) ) ;
#2178 = CARTESIAN_POINT ( 'NONE',  ( -16.60513711880302878, 100.0000000000000000, 15.15667007515659570 ) ) ;
#2179 = EDGE_CURVE ( 'NONE', #1114, #8029, #9517, .T. ) ;
#2180 = CARTESIAN_POINT ( 'NONE',  ( 3.058419780146050648, 100.0000000000000000, -23.12871267107006545 ) ) ;
#2181 = CARTESIAN_POINT ( 'NONE',  ( 0.000000000000000000, -25.00000000000000000, -0.4999999999999968914 ) ) ;
#2182 = CARTESIAN_POINT ( 'NONE',  ( 1.128215178125001161, -2.690624999385482941, 1.954126010382870815 ) ) ;
#2183 = EDGE_CURVE ( 'NONE', #9074, #2028, #4644, .T. ) ;
#2184 = VERTEX_POINT ( 'NONE', #2631 ) ;
#2185 = CARTESIAN_POINT ( 'NONE',  ( -21.39817337045129619, 100.0000000000000142, -9.317726141196148504 ) ) ;
#2186 = CONICAL_SURFACE ( 'NONE', #6199, 2.500000000000000444, 0.08726646259971666819 ) ;
#2187 = CARTESIAN_POINT ( 'NONE',  ( 5.207032889226773875, 99.50000000000000000, -23.83708953234284778 ) ) ;
#2188 = CYLINDRICAL_SURFACE ( 'NONE', #6682, 2.499999999999999556 ) ;
#2189 = CARTESIAN_POINT ( 'NONE',  ( 0.000000000000000000, 0.000000000000000000, 0.000000000000000000 ) ) ;
#2190 = ORIENTED_EDGE ( 'NONE', *, *, #2409, .T. ) ;
#2191 = B_SPLINE_CURVE_WITH_KNOTS ( 'NONE', 3,
 ( #5025, #9165, #5820, #2580, #9891, #4977, #7588, #5128, #8222, #9841, #5773, #8328, #1158, #426, #220, #8964, #7382, #2674, #1830 ),
 .UNSPECIFIED., .F., .F.,
 ( 4, 1, 1, 1, 1, 1, 1, 1, 1, 1, 1, 1, 1, 1, 1, 1, 4 ),
 ( 0.000000000000000000, 0.06485467887857676583, 0.1277145915909605745, 0.1892127134908106190, 0.2497332716026948729, 0.3109554005383074471, 0.3726238983726959941, 0.4350931267523188151, 0.5000867325104639827, 0.5644742510850394579, 0.6276292343746815439, 0.6888483565510189477, 0.7500704854866314664, 0.8105910435985150819, 0.8724026516570742018, 0.9351453211214243444, 1.000000000000000000 ),
 .UNSPECIFIED. ) ;
#2192 = DIRECTION ( 'NONE',  ( 0.000000000000000000, 1.000000000000000000, 0.000000000000000000 ) ) ;
#2193 = CARTESIAN_POINT ( 'NONE',  ( 0.000000000000000000, 0.000000000000000000, 0.000000000000000000 ) ) ;
#2194 = ORIENTED_EDGE ( 'NONE', *, *, #7603, .F. ) ;
#2195 = CARTESIAN_POINT ( 'NONE',  ( -1.767625397874844694E-16, -3.712499999999999467, -2.886751345948128655 ) ) ;
#2196 = PRODUCT_CONTEXT ( 'NONE', #7453, 'mechanical' ) ;
#2197 = CARTESIAN_POINT ( 'NONE',  ( 3.428579745388047328, 99.49999999999998579, -21.16399209792802694 ) ) ;
#2198 = CARTESIAN_POINT ( 'NONE',  ( 2.256430356250000102, -0.9281249993854827629, -2.763330213280484622E-16 ) ) ;
#2199 = CARTESIAN_POINT ( 'NONE',  ( 4.887668416326221177, 99.50000000000001421, -23.70513093767710089 ) ) ;
#2200 = CARTESIAN_POINT ( 'NONE',  ( 1.679787559701184688E-15, 2.949999998907525178, -27.43301270000000258 ) ) ;
#2201 = CARTESIAN_POINT ( 'NONE',  ( -16.49882833452567965, 100.0000000000000000, 15.05677840364783115 ) ) ;
#2202 = AXIS2_PLACEMENT_3D ( 'NONE', #5308, #9280, #1331 ) ;
#2203 = CARTESIAN_POINT ( 'NONE',  ( 0.000000000000000000, -5.000000000000000000, 0.000000000000000000 ) ) ;
#2204 = CARTESIAN_POINT ( 'NONE',  ( -16.61132721736409934, 99.50000000000001421, 16.61681399495993716 ) ) ;
#2205 = DIRECTION ( 'NONE',  ( -0.9851965920526258857, 0.000000000000000000, -0.1714283378204774222 ) ) ;
#2206 = CARTESIAN_POINT ( 'NONE',  ( -1.595409442497313560E-16, -0.2531249993854829961, -2.605501347177161087 ) ) ;
#2207 = CARTESIAN_POINT ( 'NONE',  ( 4.118246196500586542, 99.99999999999998579, -21.10643963665684453 ) ) ;
#2208 = ORIENTED_EDGE ( 'NONE', *, *, #6691, .T. ) ;
#2209 = DIRECTION ( 'NONE',  ( 0.000000000000000000, 1.000000000000000000, 0.000000000000000000 ) ) ;
#2210 = CARTESIAN_POINT ( 'NONE',  ( 19.39806930854667399, 0.9499999989075252893, 19.39806930854668465 ) ) ;
#2211 = ORIENTED_EDGE ( 'NONE', *, *, #7162, .F. ) ;
#2212 = CARTESIAN_POINT ( 'NONE',  ( -3.486133158594716510E-16, -2.756249998770965437, -2.500000000000000000 ) ) ;
#2213 = VECTOR ( 'NONE', #3036, 1000.000000000000000 ) ;
#2214 = CARTESIAN_POINT ( 'NONE',  ( 27.00000000000000355, 2.400000000000000355, 0.000000000000000000 ) ) ;
#2215 = CARTESIAN_POINT ( 'NONE',  ( 8.612131858919537919, 100.0000000000000142, 19.96100069886393413 ) ) ;
#2216 = ORIENTED_EDGE ( 'NONE', *, *, #1609, .T. ) ;
#2217 = ORIENTED_EDGE ( 'NONE', *, *, #445, .F. ) ;
#2218 = CARTESIAN_POINT ( 'NONE',  ( -15.10687288066601930, 99.49999999999998579, 15.84109048427130517 ) ) ;
#2219 = CARTESIAN_POINT ( 'NONE',  ( -15.69015368034045643, 99.50000000000001421, 16.64011368054243434 ) ) ;
#2220 = CARTESIAN_POINT ( 'NONE',  ( 1.128215178124999607, -3.103124999385482585, -1.954126010382871259 ) ) ;
#2221 = ORIENTED_EDGE ( 'NONE', *, *, #722, .F. ) ;
#2222 = ORIENTED_EDGE ( 'NONE', *, *, #3890, .T. ) ;
#2223 = VECTOR ( 'NONE', #3534, 1000.000000000000000 ) ;
#2224 = EDGE_CURVE ( 'NONE', #1392, #7177, #1871, .T. ) ;
#2225 = CARTESIAN_POINT ( 'NONE',  ( 1.045839947578414805E-15, -0.5625000000000001110, -2.500000000000000000 ) ) ;
#2226 = CARTESIAN_POINT ( 'NONE',  ( -21.59424432678268957, 99.49999999999997158, -9.639623801236600897 ) ) ;
#2227 = CARTESIAN_POINT ( 'NONE',  ( 2.256430356250000546, -0.5156249993854828961, 1.302750673588579877 ) ) ;
#2228 = CARTESIAN_POINT ( 'NONE',  ( 4.772556553149396308, 100.0000000000000000, -24.49721679606612312 ) ) ;
#2229 = VECTOR ( 'NONE', #4667, 1000.000000000000227 ) ;
#2230 = CARTESIAN_POINT ( 'NONE',  ( 5.302876193624534821E-16, -2.531249998770965348, 2.886751345948128655 ) ) ;
#2231 = VERTEX_POINT ( 'NONE', #8277 ) ;
#2232 = ADVANCED_FACE ( 'NONE', ( #9792 ), #1106, .T. ) ;
#2233 = CARTESIAN_POINT ( 'NONE',  ( 4.232798786556307036, 99.50000000000000000, -24.34936571594186105 ) ) ;
#2234 = ORIENTED_EDGE ( 'NONE', *, *, #368, .F. ) ;
#2235 = MECHANICAL_DESIGN_GEOMETRIC_PRESENTATION_REPRESENTATION (  '', ( #6248 ), #7465 ) ;
#2236 = CARTESIAN_POINT ( 'NONE',  ( 1.034219503716432668E-14, -4.162500000000000533, -2.500000000000000000 ) ) ;
#2237 = CARTESIAN_POINT ( 'NONE',  ( 4.786228327491941173E-16, -2.728124999385482585, 2.605501347177161087 ) ) ;
#2238 = EDGE_CURVE ( 'NONE', #10097, #3601, #324, .T. ) ;
#2239 = VERTEX_POINT ( 'NONE', #1832 ) ;
#2240 = DIRECTION ( 'NONE',  ( -0.2892158999609669712, 0.000000000000000000, -0.9572638942369904314 ) ) ;
#2241 = CARTESIAN_POINT ( 'NONE',  ( 0.000000000000000000, -25.00000000000000000, 0.000000000000000000 ) ) ;
#2242 = EDGE_CURVE ( 'NONE', #7345, #6501, #8011, .T. ) ;
#2243 = DIRECTION ( 'NONE',  ( 0.000000000000000000, 0.000000000000000000, -1.000000000000000000 ) ) ;
#2244 = CARTESIAN_POINT ( 'NONE',  ( 0.000000000000000000, 5.000000000000000000, -27.00000000000000000 ) ) ;
#2245 = ORIENTED_EDGE ( 'NONE', *, *, #6517, .F. ) ;
#2246 = EDGE_CURVE ( 'NONE', #9118, #369, #2749, .T. ) ;
#2247 = CARTESIAN_POINT ( 'NONE',  ( -16.63177974700816009, 99.50000000000000000, 16.59747536361813403 ) ) ;
#2248 = DIRECTION ( 'NONE',  ( 0.000000000000000000, 0.000000000000000000, -1.000000000000000000 ) ) ;
#2249 = ORIENTED_EDGE ( 'NONE', *, *, #2224, .T. ) ;
#2250 = CARTESIAN_POINT ( 'NONE',  ( -1.915120254295647584, -5.000523192925936833, -1.606958123781256464 ) ) ;
#2251 = EDGE_CURVE ( 'NONE', #8788, #9797, #4200, .T. ) ;
#2252 = DIRECTION ( 'NONE',  ( 0.7660496434811018274, 0.000000000000000000, 0.6427814120853811986 ) ) ;
#2253 = CARTESIAN_POINT ( 'NONE',  ( -1.128215178125000273, -1.228124999385483029, -1.954126010382871259 ) ) ;
#2254 = CARTESIAN_POINT ( 'NONE',  ( 1.679787559701184688E-15, 2.149999998907525356, -27.43301270000000258 ) ) ;
#2255 = ORIENTED_EDGE ( 'NONE', *, *, #6056, .F. ) ;
#2256 = CARTESIAN_POINT ( 'NONE',  ( -15.10382517959271098, 99.99999999999995737, 15.91526905993627317 ) ) ;
#2257 = VECTOR ( 'NONE', #7383, 1000.000000000000000 ) ;
#2258 = CARTESIAN_POINT ( 'NONE',  ( 4.054941747578200584, 99.99999999999998579, -24.36678493958047298 ) ) ;
#2259 = DIRECTION ( 'NONE',  ( 0.000000000000000000, 1.000000000000000000, 0.000000000000000000 ) ) ;
#2260 = B_SPLINE_SURFACE_WITH_KNOTS ( 'NONE', 3, 1, ( 
 ( #8845, #8008 ),
 ( #840, #4646 ),
 ( #6434, #6382 ),
 ( #3340, #7116 ),
 ( #4031, #7315 ),
 ( #2355, #7213 ),
 ( #4866, #9575 ),
 ( #9718, #4080 ),
 ( #5552, #6531 ),
 ( #8744, #3247 ),
 ( #1568, #8109 ) ),
 .UNSPECIFIED., .F., .F., .F.,
 ( 4, 1, 1, 1, 1, 1, 1, 1, 4 ),
 ( 2, 2 ),
 ( 0.000000000000000000, 0.09767211715481777246, 0.1989896052561311024, 0.3043518128873296535, 0.4150874769980872347, 0.5363819683935961979, 0.6738601886791220075, 0.8283091006677448798, 1.000000000000000000 ),
 ( 0.000000000000000000, 1.000000000000000000 ),
 .UNSPECIFIED. ) ;
#2261 = EDGE_CURVE ( 'NONE', #9021, #519, #7740, .T. ) ;
#2262 = CARTESIAN_POINT ( 'NONE',  ( -15.84348323231452049, 100.0000000000000000, 15.18005498687102772 ) ) ;
#2263 = CARTESIAN_POINT ( 'NONE',  ( 4.786228327491940187E-16, -0.4781249993854829183, 2.605501347177161087 ) ) ;
#2264 = CARTESIAN_POINT ( 'NONE',  ( 3.771794781161601939, 99.49999999999998579, -21.07813736596861176 ) ) ;
#2265 = ORIENTED_EDGE ( 'NONE', *, *, #2685, .T. ) ;
#2266 = CARTESIAN_POINT ( 'NONE',  ( -2.256430356250000102, -2.428124999385482319, -1.302750673588580321 ) ) ;
#2267 = CARTESIAN_POINT ( 'NONE',  ( -27.43301270000000969, 2.299999998907525267, 11.36312591709335429 ) ) ;
#2268 =( LENGTH_UNIT ( ) NAMED_UNIT ( * ) SI_UNIT ( .MILLI., .METRE. ) );
#2269 = CARTESIAN_POINT ( 'NONE',  ( 0.000000000000000000, 100.0000000000000000, -27.00000000000000355 ) ) ;
#2270 = APPLICATION_CONTEXT ( 'automotive_design' ) ;
#2271 = CARTESIAN_POINT ( 'NONE',  ( -11.18376618407358336, 0.5500000000000000444, 26.99999999999999645 ) ) ;
#2272 = CARTESIAN_POINT ( 'NONE',  ( 9.357295078982289738, 99.50000000000004263, 20.12145687760884627 ) ) ;
#2273 = ORIENTED_EDGE ( 'NONE', *, *, #6979, .T. ) ;
#2274 = AXIS2_PLACEMENT_3D ( 'NONE', #2759, #7404, #3382 ) ;
#2275 = ORIENTED_EDGE ( 'NONE', *, *, #6709, .F. ) ;
#2276 = CARTESIAN_POINT ( 'NONE',  ( -16.49092618789450526, 99.50000000000000000, 16.26472549871478179 ) ) ;
#2277 = CARTESIAN_POINT ( 'NONE',  ( 8.091962505948220752, 99.99999999999995737, 20.48385654212622242 ) ) ;
#2278 = CARTESIAN_POINT ( 'NONE',  ( -2.256430356249999214, -4.265624999385482674, 1.302750673588581876 ) ) ;
#2279 = ORIENTED_EDGE ( 'NONE', *, *, #562, .T. ) ;
#2280 = VERTEX_POINT ( 'NONE', #1354 ) ;
#2281 = CARTESIAN_POINT ( 'NONE',  ( -27.43301270000000258, 3.799999998907525711, -11.36312591709336317 ) ) ;
#2282 = CARTESIAN_POINT ( 'NONE',  ( 2.256430356249999658, -1.340624999385482852, -1.302750673588581432 ) ) ;
#2283 = CARTESIAN_POINT ( 'NONE',  ( 5.242860087038358152, 100.0000000000000568, -23.52699316036146371 ) ) ;
#2284 = CARTESIAN_POINT ( 'NONE',  ( -0.6698729810778054627, -1.707596189432333933, 2.500000000000000000 ) ) ;
#2285 = AXIS2_PLACEMENT_3D ( 'NONE', #660, #5534, #3026 ) ;
#2286 = ORIENTED_EDGE ( 'NONE', *, *, #9968, .T. ) ;
#2287 = CARTESIAN_POINT ( 'NONE',  ( -1.249999999999998224, -1.218749998770965792, 2.165063509461097713 ) ) ;
#2288 = ORIENTED_EDGE ( 'NONE', *, *, #8558, .F. ) ;
#2289 = VECTOR ( 'NONE', #4116, 1000.000000000000000 ) ;
#2290 = CARTESIAN_POINT ( 'NONE',  ( -10.49999999999999822, 104.5000000000000142, 0.000000000000000000 ) ) ;
#2291 = CARTESIAN_POINT ( 'NONE',  ( -16.01161620991261358, 99.50000000000000000, 17.10240122391520146 ) ) ;
#2292 = CARTESIAN_POINT ( 'NONE',  ( 9.263267005978743640, 99.49999999999998579, 19.65676951151765905 ) ) ;
#2293 = CARTESIAN_POINT ( 'NONE',  ( -1.128215178124998497, -1.865624999385482763, 1.954126010382872147 ) ) ;
#2294 = EDGE_CURVE ( 'NONE', #1242, #8813, #2753, .T. ) ;
#2295 = ORIENTED_EDGE ( 'NONE', *, *, #5584, .T. ) ;
#2296 = CARTESIAN_POINT ( 'NONE',  ( 2.983739933759421259, 99.49999999999998579, -23.28421226151478152 ) ) ;
#2297 = AXIS2_PLACEMENT_3D ( 'NONE', #4641, #2120, #7834 ) ;
#2298 = CARTESIAN_POINT ( 'NONE',  ( 9.526349065647009340, 99.50000000000000000, 19.81320455978211470 ) ) ;
#2299 = CARTESIAN_POINT ( 'NONE',  ( 0.000000000000000000, 100.0000000000000000, -25.00000000000000000 ) ) ;
#2300 = CARTESIAN_POINT ( 'NONE',  ( -16.35834224700816009, 99.50000000000000000, 16.43761959438736397 ) ) ;
#2301 = ORIENTED_EDGE ( 'NONE', *, *, #2676, .F. ) ;
#2302 = CARTESIAN_POINT ( 'NONE',  ( -27.00000000000000355, 2.599999997815050534, -3.306546357697854128E-15 ) ) ;
#2303 = CARTESIAN_POINT ( 'NONE',  ( -11.36312591709337561, 4.899999998907527576, 27.43301269999999548 ) ) ;
#2304 = CARTESIAN_POINT ( 'NONE',  ( -1.249999999999998224, -3.974999999999999201, 2.165063509461097713 ) ) ;
#2305 = CARTESIAN_POINT ( 'NONE',  ( -20.99557965837879081, 99.99999999999997158, -10.74478602187354959 ) ) ;
#2306 = CARTESIAN_POINT ( 'NONE',  ( 1.128215178124999607, -4.453124999385482674, -1.954126010382871259 ) ) ;
#2307 = CARTESIAN_POINT ( 'NONE',  ( -16.62994343074595349, 99.49999999999998579, 15.18287566599475191 ) ) ;
#2308 = CARTESIAN_POINT ( 'NONE',  ( -27.43301270000000258, 3.899999998907525356, -11.36312591709336317 ) ) ;
#2309 = DIRECTION ( 'NONE',  ( 0.000000000000000000, 1.000000000000000000, 0.000000000000000000 ) ) ;
#2310 = DIRECTION ( 'NONE',  ( -0.9198211419112228837, 0.000000000000000000, 0.3923379498508065000 ) ) ;
#2311 = CARTESIAN_POINT ( 'NONE',  ( 8.132491713109025966, 100.0000000000000000, 21.08089001807756091 ) ) ;
#2312 = CARTESIAN_POINT ( 'NONE',  ( -22.58826642033182353, 99.99999999999998579, -9.883148377786627137 ) ) ;
#2313 = CARTESIAN_POINT ( 'NONE',  ( 2.256430356250000102, -3.515624999385482674, -2.763330213280484622E-16 ) ) ;
#2314 = CARTESIAN_POINT ( 'NONE',  ( 4.570993444255353921, 99.49999999999998579, -21.37574484917381668 ) ) ;
#2315 = EDGE_LOOP ( 'NONE', ( #639, #1193, #9766, #6001, #7882, #10359, #3137, #9438, #1307, #1744, #3858, #1327, #6004, #7273, #3797, #5535 ) ) ;
#2316 = CARTESIAN_POINT ( 'NONE',  ( -1.128215178124998497, -2.315624999385482941, 1.954126010382872147 ) ) ;
#2317 = CARTESIAN_POINT ( 'NONE',  ( 19.39806930854668110, 1.249999998907525223, -19.39806930854668110 ) ) ;
#2318 = EDGE_CURVE ( 'NONE', #5272, #1184, #243, .T. ) ;
#2319 = CARTESIAN_POINT ( 'NONE',  ( -15.56505537928961047, 99.50000000000002842, 14.87309967080592088 ) ) ;
#2320 = EDGE_CURVE ( 'NONE', #2411, #600, #3373, .T. ) ;
#2321 = CARTESIAN_POINT ( 'NONE',  ( 19.09188309203678102, 0.6999999999999999556, 19.09188309203678813 ) ) ;
#2322 = CARTESIAN_POINT ( 'NONE',  ( 8.829292973371666520, 100.0000000000000142, 19.92220432019063736 ) ) ;
#2323 = EDGE_LOOP ( 'NONE', ( #7748, #7808, #9311, #9330, #5771, #8232, #4312, #4481 ) ) ;
#2324 = SHAPE_REPRESENTATION ( 'lid', ( #5055 ), #7565 ) ;
#2325 = CARTESIAN_POINT ( 'NONE',  ( -16.57337958714257908, 99.49999999999998579, 15.99273699073067867 ) ) ;
#2326 = CARTESIAN_POINT ( 'NONE',  ( -15.55395551812965671, 99.50000000000002842, 16.59868653893595791 ) ) ;
#2327 = VERTEX_POINT ( 'NONE', #9233 ) ;
#2328 = CARTESIAN_POINT ( 'NONE',  ( 2.256430356250000546, -4.565624999385482496, 1.302750673588579877 ) ) ;
#2329 = ORIENTED_EDGE ( 'NONE', *, *, #9518, .F. ) ;
#2330 = CARTESIAN_POINT ( 'NONE',  ( -19.39806930854667755, 1.349999998907525534, -19.39806930854668110 ) ) ;
#2331 = CARTESIAN_POINT ( 'NONE',  ( 3.701176614148623756, 100.0000000000000000, -24.64875008328975170 ) ) ;
#2332 = CARTESIAN_POINT ( 'NONE',  ( 2.256430356249999658, -2.240624999385482319, -1.302750673588581432 ) ) ;
#2333 = CARTESIAN_POINT ( 'NONE',  ( 2.143131898507868643E-15, 97.00000000000000000, 17.50000000000000355 ) ) ;
#2334 = PLANE ( 'NONE',  #4109 ) ;
#2335 = PLANE ( 'NONE',  #2285 ) ;
#2336 = CARTESIAN_POINT ( 'NONE',  ( 2.500000000000000000, -2.868749998770965703, -3.061616997868383141E-16 ) ) ;
#2337 = ORIENTED_EDGE ( 'NONE', *, *, #3309, .T. ) ;
#2338 = CARTESIAN_POINT ( 'NONE',  ( 4.118246196500586542, 99.99999999999998579, -21.10643963665684453 ) ) ;
#2339 = CARTESIAN_POINT ( 'NONE',  ( 4.739008722453744049, 99.50000000000001421, -24.06821587619827696 ) ) ;
#2340 = DIRECTION ( 'NONE',  ( 0.000000000000000000, -1.000000000000000000, 0.000000000000000000 ) ) ;
#2341 = CARTESIAN_POINT ( 'NONE',  ( 2.256430356250000546, -1.303124999385482985, 1.302750673588579877 ) ) ;
#2342 = B_SPLINE_SURFACE_WITH_KNOTS ( 'NONE', 3, 1, ( 
 ( #8056, #9676 ),
 ( #2514, #5705 ),
 ( #1718, #4912 ),
 ( #2560, #5752 ),
 ( #1517, #4710 ),
 ( #7903, #7459 ),
 ( #1909, #9141 ),
 ( #1809, #2653 ),
 ( #6673, #5001 ),
 ( #7358, #8301 ),
 ( #1031, #1132 ),
 ( #1185, #9091 ),
 ( #984, #4325 ),
 ( #4376, #8201 ),
 ( #5101, #199 ) ),
 .UNSPECIFIED., .F., .F., .F.,
 ( 4, 1, 1, 1, 1, 1, 1, 1, 1, 1, 1, 1, 4 ),
 ( 2, 2 ),
 ( 0.000000000000000000, 0.1055296353700490852, 0.2070742529895955586, 0.3056622059958778448, 0.4023599870273183998, 0.4943057198019382148, 0.5778637904027289496, 0.6550095244395398586, 0.7278863574113029200, 0.7976678238154090161, 0.8645871040366396310, 0.9319858836656568224, 1.000000000000000000 ),
 ( 0.000000000000000000, 1.000000000000000000 ),
 .UNSPECIFIED. ) ;
#2343 = ORIENTED_EDGE ( 'NONE', *, *, #10127, .T. ) ;
#2344 = CARTESIAN_POINT ( 'NONE',  ( -22.28738277804067636, 99.99999999999997158, -10.06255608345902886 ) ) ;
#2345 = DIRECTION ( 'NONE',  ( 0.000000000000000000, 0.000000000000000000, 1.000000000000000000 ) ) ;
#2346 = CARTESIAN_POINT ( 'NONE',  ( -18.01369080470046313, 99.50000000000000000, 17.15556831233607937 ) ) ;
#2347 = FACE_OUTER_BOUND ( 'NONE', #5980, .T. ) ;
#2348 = CARTESIAN_POINT ( 'NONE',  ( 27.43301269999999548, 3.499999998907525445, 11.36312591709337916 ) ) ;
#2349 = ORIENTED_EDGE ( 'NONE', *, *, #3197, .T. ) ;
#2350 = EDGE_CURVE ( 'NONE', #6922, #2378, #7401, .T. ) ;
#2351 = CARTESIAN_POINT ( 'NONE',  ( -1.250000000000000222, -3.224999999999999645, -2.165063509461096825 ) ) ;
#2352 = VECTOR ( 'NONE', #2815, 1000.000000000000000 ) ;
#2353 = CARTESIAN_POINT ( 'NONE',  ( -20.91264567078791714, 99.99999999999997158, -10.54226115003387676 ) ) ;
#2354 = CARTESIAN_POINT ( 'NONE',  ( -1.128215178125000273, -3.478124999385482141, -1.954126010382871259 ) ) ;
#2355 = CARTESIAN_POINT ( 'NONE',  ( -20.79740905086423552, 99.50000000000001421, -11.06234285579171051 ) ) ;
#2356 = CARTESIAN_POINT ( 'NONE',  ( -27.43301270000000258, 4.699999998907525622, -11.36312591709336317 ) ) ;
#2357 = CARTESIAN_POINT ( 'NONE',  ( -15.15871127190382417, 99.99999999999997158, 15.63231653451427761 ) ) ;
#2358 = CARTESIAN_POINT ( 'NONE',  ( 11.18376618407357626, 3.649999997815050357, 27.00000000000000000 ) ) ;
#2359 = CARTESIAN_POINT ( 'NONE',  ( 21.43339342948717885, 99.50000000000000000, -1.392427884615384803 ) ) ;
#2360 = ADVANCED_FACE ( 'NONE', ( #9865 ), #1026, .F. ) ;
#2361 = CARTESIAN_POINT ( 'NONE',  ( 3.061616997868382648E-16, 0.000000000000000000, 2.499999999999999556 ) ) ;
#2362 = CARTESIAN_POINT ( 'NONE',  ( -2.256430356250000102, -4.228124999385483029, -1.302750673588580321 ) ) ;
#2363 = CARTESIAN_POINT ( 'NONE',  ( 4.691018317478480526, 99.49999999999995737, -21.52316599815148024 ) ) ;
#2364 = EDGE_CURVE ( 'NONE', #4614, #9350, #720, .T. ) ;
#2365 = CARTESIAN_POINT ( 'NONE',  ( -2.256430356250000102, -3.328124999385483562, -1.302750673588580321 ) ) ;
#2366 = CARTESIAN_POINT ( 'NONE',  ( 19.39806930854668110, 0.4499999989075251783, -19.39806930854668110 ) ) ;
#2367 = CARTESIAN_POINT ( 'NONE',  ( 3.061616997868383141E-16, 0.000000000000000000, 2.500000000000000000 ) ) ;
#2368 = CARTESIAN_POINT ( 'NONE',  ( -11.18376618407358336, 4.549999999999999822, 26.99999999999999645 ) ) ;
#2369 = CARTESIAN_POINT ( 'NONE',  ( 3.195700652717397894, 99.99999999999997158, -22.66286045753255962 ) ) ;
#2370 = EDGE_CURVE ( 'NONE', #10090, #7760, #5993, .T. ) ;
#2371 = ORIENTED_EDGE ( 'NONE', *, *, #5557, .F. ) ;
#2372 = PRODUCT_DEFINITION ( 'UNKNOWN', '', #6143, #4664 ) ;
#2373 = FILL_AREA_STYLE_COLOUR ( '', #1153 ) ;
#2374 = CARTESIAN_POINT ( 'NONE',  ( -15.33577160963320374, 99.99999999999998579, 16.45272793336155814 ) ) ;
#2375 = ADVANCED_FACE ( 'NONE', ( #4272 ), #5566, .F. ) ;
#2376 = ORIENTED_EDGE ( 'NONE', *, *, #3307, .T. ) ;
#2377 = CARTESIAN_POINT ( 'NONE',  ( 2.256430356249999658, -4.940624999385482496, -1.302750673588581432 ) ) ;
#2378 = VERTEX_POINT ( 'NONE', #7452 ) ;
#2379 = EDGE_CURVE ( 'NONE', #2983, #3142, #2506, .T. ) ;
#2380 = CARTESIAN_POINT ( 'NONE',  ( -11.36312591709335962, 1.299999998907525267, -27.43301270000000258 ) ) ;
#2381 = CARTESIAN_POINT ( 'NONE',  ( -9.703070624755296135E-15, -4.331249998770966059, 2.500000000000000444 ) ) ;
#2382 = CIRCLE ( 'NONE', #2018, 2.500000000000000000 ) ;
#2383 = CARTESIAN_POINT ( 'NONE',  ( -22.22752541189434794, 99.49999999999994316, -11.26717589342885084 ) ) ;
#2384 = CARTESIAN_POINT ( 'NONE',  ( 4.786228327491940187E-16, -3.740624999385481875, 2.605501347177161087 ) ) ;
#2385 = CARTESIAN_POINT ( 'NONE',  ( -27.00000000000000355, 1.749999997815050445, -11.18376618407357270 ) ) ;
#2386 = EDGE_CURVE ( 'NONE', #2471, #2404, #7063, .T. ) ;
#2387 = CARTESIAN_POINT ( 'NONE',  ( -16.81182640597031508, 100.0000000000000000, 16.36129326314865295 ) ) ;
#2388 = CARTESIAN_POINT ( 'NONE',  ( 4.363164797760430424, 99.50000000000002842, -21.67376679147534446 ) ) ;
#2389 =( BOUNDED_CURVE ( )  B_SPLINE_CURVE ( 2, ( #10046, #5910, #4342, #9944, #2778, #5285, #4447, #9058, #475 ),
 .UNSPECIFIED., .F., .F. ) 
 B_SPLINE_CURVE_WITH_KNOTS ( ( 3, 2, 2, 2, 3 ),
 ( 0.6071428571428570953, 0.6250000000000000000, 0.6428571428571429047, 0.6607142857142856984, 0.6785714285714286031 ),
 .UNSPECIFIED. ) 
 CURVE ( )  GEOMETRIC_REPRESENTATION_ITEM ( )  RATIONAL_B_SPLINE_CURVE ( ( 1.000000000000000000, 0.9238795325112867385, 1.000000000000000000, 0.9238795325112867385, 1.000000000000000000, 0.9238795325112867385, 1.000000000000000000, 0.9238795325112867385, 1.000000000000000000 ) ) 
 REPRESENTATION_ITEM ( '' )  );
#2390 = AXIS2_PLACEMENT_3D ( 'NONE', #4355, #2048, #7538 ) ;
#2391 = CARTESIAN_POINT ( 'NONE',  ( 2.500000000000000444, -1.106249998770965748, 1.443375672974063439 ) ) ;
#2392 = ORIENTED_EDGE ( 'NONE', *, *, #10016, .T. ) ;
#2393 = DIRECTION ( 'NONE',  ( 0.7071067811865473507, 0.000000000000000000, 0.7071067811865477948 ) ) ;
#2394 = CARTESIAN_POINT ( 'NONE',  ( 0.000000000000000000, 105.0000000000000142, -17.50000000000000355 ) ) ;
#2395 = CARTESIAN_POINT ( 'NONE',  ( -15.03963071504896121, 100.0000000000000142, 16.63526396357264758 ) ) ;
#2396 = CARTESIAN_POINT ( 'NONE',  ( 2.256430356250000546, -4.003124999385482496, 1.302750673588579877 ) ) ;
#2397 = VECTOR ( 'NONE', #686, 1000.000000000000000 ) ;
#2398 = VERTEX_POINT ( 'NONE', #2858 ) ;
#2399 = CARTESIAN_POINT ( 'NONE',  ( -22.00707282958688182, 99.99999999999997158, -9.748971510896797810 ) ) ;
#2400 = CARTESIAN_POINT ( 'NONE',  ( -22.34945848979098670, 99.50000000000002842, -10.27225542379191481 ) ) ;
#2401 = FACE_OUTER_BOUND ( 'NONE', #8600, .T. ) ;
#2402 = VECTOR ( 'NONE', #3750, 1000.000000000000114 ) ;
#2403 = CARTESIAN_POINT ( 'NONE',  ( -27.43301270000000258, 3.949999998907525178, -3.359575119402369376E-15 ) ) ;
#2404 = VERTEX_POINT ( 'NONE', #5098 ) ;
#2405 = CARTESIAN_POINT ( 'NONE',  ( -1.250000000000000222, -3.674999999999999822, -2.165063509461096825 ) ) ;
#2406 = CARTESIAN_POINT ( 'NONE',  ( 2.256430356250000546, -4.565624999385482496, 1.302750673588579877 ) ) ;
#2407 = CARTESIAN_POINT ( 'NONE',  ( -20.91430522584054330, 99.50000000000001421, -10.19152558580213608 ) ) ;
#2408 = CARTESIAN_POINT ( 'NONE',  ( -19.09188309203678813, 1.099999997815050312, 19.09188309203678457 ) ) ;
#2409 = EDGE_CURVE ( 'NONE', #2184, #9074, #2098, .T. ) ;
#2410 = CARTESIAN_POINT ( 'NONE',  ( -15.22739782325755442, 99.99999999999995737, 15.50750051783781025 ) ) ;
#2411 = VERTEX_POINT ( 'NONE', #1076 ) ;
#2412 = CARTESIAN_POINT ( 'NONE',  ( -16.18394139941567644, 99.50000000000000000, 16.57042731130403723 ) ) ;
#2413 = CARTESIAN_POINT ( 'NONE',  ( 26.99999999999999645, 3.950000000000000178, 11.18376618407358691 ) ) ;
#2414 = CARTESIAN_POINT ( 'NONE',  ( -2.256430356250000102, -3.328124999385483562, -1.302750673588580321 ) ) ;
#2415 = CARTESIAN_POINT ( 'NONE',  ( 4.202475441399873723, 99.50000000000000000, -24.35385978717689071 ) ) ;
#2416 = ORIENTED_EDGE ( 'NONE', *, *, #7857, .F. ) ;
#2417 = CARTESIAN_POINT ( 'NONE',  ( 4.786228327491941173E-16, -2.728124999385482585, 2.605501347177161087 ) ) ;
#2418 = CARTESIAN_POINT ( 'NONE',  ( -27.43301270000000969, 0.7999999989075252671, 11.36312591709335429 ) ) ;
#2419 = SURFACE_SIDE_STYLE ('',( #7075 ) ) ;
#2420 = CARTESIAN_POINT ( 'NONE',  ( -3.486133158594716510E-16, -1.012499999999999956, -2.500000000000000000 ) ) ;
#2421 = CARTESIAN_POINT ( 'NONE',  ( -11.18376618407358336, 2.950000000000000178, 26.99999999999999645 ) ) ;
#2422 = FACE_OUTER_BOUND ( 'NONE', #1938, .T. ) ;
#2423 = EDGE_CURVE ( 'NONE', #3612, #1790, #9034, .T. ) ;
#2424 = DIRECTION ( 'NONE',  ( 0.000000000000000000, 0.000000000000000000, -1.000000000000000000 ) ) ;
#2425 = CARTESIAN_POINT ( 'NONE',  ( -20.95611194834973645, 99.50000000000000000, -10.07788454426966318 ) ) ;
#2426 = VERTEX_POINT ( 'NONE', #4320 ) ;
#2427 = CARTESIAN_POINT ( 'NONE',  ( -2.256430356249999214, -4.715624999385481964, 1.302750673588581876 ) ) ;
#2428 = ORIENTED_EDGE ( 'NONE', *, *, #121, .F. ) ;
#2429 = CARTESIAN_POINT ( 'NONE',  ( -19.39806930854667755, 2.149999998907525356, -19.39806930854668110 ) ) ;
#2430 = CARTESIAN_POINT ( 'NONE',  ( 3.171774962637509798, 99.50000000000000000, -24.28498992023182268 ) ) ;
#2431 = PRODUCT_DEFINITION_SHAPE ( 'NONE', 'NONE',  #2680 ) ;
#2432 = DIRECTION ( 'NONE',  ( 0.9985288298541962204, 0.000000000000000000, -0.05422338932609765960 ) ) ;
#2433 = CARTESIAN_POINT ( 'NONE',  ( 2.256430356249999658, -4.940624999385482496, -1.302750673588581432 ) ) ;
#2434 = CARTESIAN_POINT ( 'NONE',  ( -16.57337958714257908, 99.99999999999998579, 15.99273699073067867 ) ) ;
#2435 = AXIS2_PLACEMENT_3D ( 'NONE', #6046, #2240, #5383 ) ;
#2436 = CARTESIAN_POINT ( 'NONE',  ( -22.67341330918043951, 99.50000000000000000, -10.57563951594260665 ) ) ;
#2437 = CARTESIAN_POINT ( 'NONE',  ( 4.850954546176396320, 99.99999999999998579, -24.43907202982397209 ) ) ;
#2438 = EDGE_LOOP ( 'NONE', ( #1622, #7880, #10051, #8233 ) ) ;
#2439 = CARTESIAN_POINT ( 'NONE',  ( 2.500000000000000000, -1.518749998770965837, -3.061616997868383141E-16 ) ) ;
#2440 = ORIENTED_EDGE ( 'NONE', *, *, #10080, .T. ) ;
#2441 = AXIS2_PLACEMENT_3D ( 'NONE', #6592, #8319, #953 ) ;
#2442 = CARTESIAN_POINT ( 'NONE',  ( 4.693123912524271191, 99.50000000000002842, -24.12247278045041554 ) ) ;
#2443 = CARTESIAN_POINT ( 'NONE',  ( -16.01161620991261358, 100.0000000000000000, 17.10240122391520146 ) ) ;
#2444 = CARTESIAN_POINT ( 'NONE',  ( 27.21650635000000307, 0.1249999994537626252, 0.000000000000000000 ) ) ;
#2445 = CARTESIAN_POINT ( 'NONE',  ( -1.728525935690056192, -5.141148612710514598, -1.450405475118361043 ) ) ;
#2446 = B_SPLINE_CURVE_WITH_KNOTS ( 'NONE', 3,
 ( #9767, #3432, #4176, #299, #8354, #5951, #5052, #3488, #9869, #9978, #1960, #6625, #6576, #5156, #2606 ),
 .UNSPECIFIED., .F., .F.,
 ( 4, 1, 1, 1, 1, 1, 1, 1, 1, 1, 1, 1, 4 ),
 ( 0.000000000000000000, 0.09895296010982183865, 0.1966578232739713550, 0.2939931048315790330, 0.3929322324600736938, 0.4463669803336778319, 0.5055752425223922764, 0.5715235163887821823, 0.6440401046887170855, 0.7229629404452876384, 0.8087840669208056221, 0.9009145765370688563, 1.000000000000000000 ),
 .UNSPECIFIED. ) ;
#2447 = ORIENTED_EDGE ( 'NONE', *, *, #322, .F. ) ;
#2448 = EDGE_CURVE ( 'NONE', #969, #8911, #5891, .T. ) ;
#2449 = CARTESIAN_POINT ( 'NONE',  ( -21.94169572595625795, 100.0000000000000000, -9.715372641902229489 ) ) ;
#2450 = ORIENTED_EDGE ( 'NONE', *, *, #9527, .F. ) ;
#2451 =( NAMED_UNIT ( * ) SI_UNIT ( $, .STERADIAN. ) SOLID_ANGLE_UNIT ( ) );
#2452 = CARTESIAN_POINT ( 'NONE',  ( -15.03963071504896121, 99.50000000000001421, 16.63526396357264758 ) ) ;
#2453 = CARTESIAN_POINT ( 'NONE',  ( 9.357295078982289738, 100.0000000000000426, 20.12145687760884627 ) ) ;
#2454 = ORIENTED_EDGE ( 'NONE', *, *, #8510, .T. ) ;
#2455 = CARTESIAN_POINT ( 'NONE',  ( 3.302864939465488536, 100.0000000000000142, -22.83905924565489443 ) ) ;
#2456 = AXIS2_PLACEMENT_3D ( 'NONE', #3728, #9207, #9110 ) ;
#2457 = CARTESIAN_POINT ( 'NONE',  ( -3.486133158594716510E-16, -0.5062499987709657701, -2.500000000000000000 ) ) ;
#2458 = CARTESIAN_POINT ( 'NONE',  ( 1.128215178124999607, -4.003124999385482496, -1.954126010382871259 ) ) ;
#2459 = CARTESIAN_POINT ( 'NONE',  ( -21.03403678956047074, 99.50000000000001421, -10.80451401317004922 ) ) ;
#2460 = CARTESIAN_POINT ( 'NONE',  ( -5.039362679103552881E-15, 4.149999998907524912, 27.43301270000000258 ) ) ;
#2461 = PRODUCT_DEFINITION_CONTEXT ( 'detailed design', #2595, 'design' ) ;
#2462 = CARTESIAN_POINT ( 'NONE',  ( -15.13520964245927836, 99.49999999999998579, 15.69931698147095034 ) ) ;
#2463 = VECTOR ( 'NONE', #7583, 1000.000000000000000 ) ;
#2464 = CARTESIAN_POINT ( 'NONE',  ( -10.49999999999999822, 105.0000000000000142, 0.000000000000000000 ) ) ;
#2465 = CARTESIAN_POINT ( 'NONE',  ( -9.703070624755296135E-15, -3.937500000000000888, 2.500000000000000444 ) ) ;
#2466 = CARTESIAN_POINT ( 'NONE',  ( -7.500000000000000888, 104.5000000000000142, 3.000000000000000000 ) ) ;
#2467 = APPLICATION_CONTEXT ( 'automotive_design' ) ;
#2468 = CARTESIAN_POINT ( 'NONE',  ( 2.256430356250000546, -2.653124999385482852, 1.302750673588579877 ) ) ;
#2469 = CARTESIAN_POINT ( 'NONE',  ( 9.881472129446523311, 100.0000000000000284, 20.94326683228310060 ) ) ;
#2470 = ORIENTED_EDGE ( 'NONE', *, *, #3419, .T. ) ;
#2471 = VERTEX_POINT ( 'NONE', #1851 ) ;
#2472 = CARTESIAN_POINT ( 'NONE',  ( -2.500000000000000000, -0.4500000000000000111, 0.000000000000000000 ) ) ;
#2473 = CARTESIAN_POINT ( 'NONE',  ( -11.36312591709335962, 1.399999998907525578, -27.43301270000000258 ) ) ;
#2474 = LINE ( 'NONE', #6542, #4925 ) ;
#2475 = CARTESIAN_POINT ( 'NONE',  ( 1.679787559701184688E-15, 0.4499999989075252338, -27.43301270000000258 ) ) ;
#2476 = CARTESIAN_POINT ( 'NONE',  ( -21.07003209069497984, 99.99999999999998579, -11.28505157174820361 ) ) ;
#2477 = PRESENTATION_LAYER_ASSIGNMENT (  '', '', ( #453 ) ) ;
#2478 = CARTESIAN_POINT ( 'NONE',  ( 0.000000000000000000, 73.81339255365637086, 0.000000000000000000 ) ) ;
#2479 = CARTESIAN_POINT ( 'NONE',  ( -21.18296228862668329, 99.50000000000002842, -10.95406920104765724 ) ) ;
#2480 = ORIENTED_EDGE ( 'NONE', *, *, #6506, .F. ) ;
#2481 = ORIENTED_EDGE ( 'NONE', *, *, #6348, .T. ) ;
#2482 = CARTESIAN_POINT ( 'NONE',  ( 2.847408871211157155, 100.0000000000000142, -22.10537533382872510 ) ) ;
#2483 = CARTESIAN_POINT ( 'NONE',  ( 2.500000000000000000, -5.081249998770965171, -1.443375672974065438 ) ) ;
#2484 = CARTESIAN_POINT ( 'NONE',  ( -27.43301270000000258, 2.199999998907525622, -11.36312591709336317 ) ) ;
#2485 = CARTESIAN_POINT ( 'NONE',  ( 1.034219503716432668E-14, -3.656249998770965792, -2.500000000000000000 ) ) ;
#2486 = EDGE_CURVE ( 'NONE', #9410, #3042, #5047, .T. ) ;
#2487 = CARTESIAN_POINT ( 'NONE',  ( -22.10910773081910818, 100.0000000000000142, -11.33820747227609793 ) ) ;
#2488 = CARTESIAN_POINT ( 'NONE',  ( 1.128215178124999607, -4.003124999385482496, -1.954126010382871259 ) ) ;
#2489 = CARTESIAN_POINT ( 'NONE',  ( -16.49092618789450526, 100.0000000000000000, 16.26472549871478179 ) ) ;
#2490 = CARTESIAN_POINT ( 'NONE',  ( -16.84090648038580085, 99.49999999999998579, 15.49469789757679727 ) ) ;
#2491 = CARTESIAN_POINT ( 'NONE',  ( 4.922541232168287983, 100.0000000000000284, -24.37252920941159928 ) ) ;
#2492 = VECTOR ( 'NONE', #6820, 1000.000000000000000 ) ;
#2493 = CARTESIAN_POINT ( 'NONE',  ( 2.500000000000000444, -4.706249998770965171, 1.443375672974063439 ) ) ;
#2494 = VERTEX_POINT ( 'NONE', #10062 ) ;
#2495 = CARTESIAN_POINT ( 'NONE',  ( 4.457146071884139360, 99.50000000000001421, -24.28472590373185724 ) ) ;
#2496 = EDGE_CURVE ( 'NONE', #6993, #5685, #2105, .T. ) ;
#2497 = CARTESIAN_POINT ( 'NONE',  ( 3.000000000000000000, -15.00000000000000000, -1.732050807568876749 ) ) ;
#2498 = CARTESIAN_POINT ( 'NONE',  ( 2.256430356249999658, -4.828124999385483562, -1.302750673588581432 ) ) ;
#2499 = ORIENTED_EDGE ( 'NONE', *, *, #4168, .T. ) ;
#2500 = EDGE_CURVE ( 'NONE', #1790, #3644, #328, .T. ) ;
#2501 = DIRECTION ( 'NONE',  ( -0.000000000000000000, -0.000000000000000000, -1.000000000000000000 ) ) ;
#2502 = VECTOR ( 'NONE', #2501, 1000.000000000000000 ) ;
#2503 = CARTESIAN_POINT ( 'NONE',  ( -1.249999999999998224, -3.524999999999999467, 2.165063509461097713 ) ) ;
#2504 = ADVANCED_FACE ( 'NONE', ( #3737 ), #5978, .T. ) ;
#2505 = CARTESIAN_POINT ( 'NONE',  ( -16.30857500771091040, 99.49999999999994316, 15.34700649443169063 ) ) ;
#2506 =( BOUNDED_CURVE ( )  B_SPLINE_CURVE ( 2, ( #6723, #2065, #5259, #1128, #5152, #10023, #5202 ),
 .UNSPECIFIED., .F., .F. ) 
 B_SPLINE_CURVE_WITH_KNOTS ( ( 3, 2, 2, 3 ),
 ( 0.8958333333333333703, 0.9027777777777777901, 0.9166666666666666297, 0.9258784821878333071 ),
 .UNSPECIFIED. ) 
 CURVE ( )  GEOMETRIC_REPRESENTATION_ITEM ( )  RATIONAL_B_SPLINE_CURVE ( ( 0.9330127018922192983, 0.9330127018922198534, 1.000000000000000000, 0.8660254037844387076, 1.000000000000000000, 0.9111412529300411123, 0.9401537613649495473 ) ) 
 REPRESENTATION_ITEM ( '' )  );
#2507 = CARTESIAN_POINT ( 'NONE',  ( -5.039362679103552881E-15, 4.949999998907525622, 27.43301270000000258 ) ) ;
#2508 = ORIENTED_EDGE ( 'NONE', *, *, #2556, .F. ) ;
#2509 = ADVANCED_FACE ( 'NONE', ( #1164 ), #1270, .T. ) ;
#2510 = CARTESIAN_POINT ( 'NONE',  ( -20.42657152723830905, 99.50000000000000000, -10.54129411626120216 ) ) ;
#2511 = CARTESIAN_POINT ( 'NONE',  ( -20.89884294283097432, 100.0000000000000142, -10.47119744953613640 ) ) ;
#2512 = CARTESIAN_POINT ( 'NONE',  ( -1.128215178124998497, -4.228124999385482141, 1.954126010382872147 ) ) ;
#2513 = ORIENTED_EDGE ( 'NONE', *, *, #3854, .F. ) ;
#2514 = CARTESIAN_POINT ( 'NONE',  ( 4.061806280070601183, 99.50000000000001421, -22.51960061163626392 ) ) ;
#2515 = CARTESIAN_POINT ( 'NONE',  ( 19.09188309203678813, 0.6999999978150504010, -19.09188309203678813 ) ) ;
#2516 = CARTESIAN_POINT ( 'NONE',  ( 7.500000000000000000, 104.5000000000000142, 1.000000000000000222 ) ) ;
#2517 = ORIENTED_EDGE ( 'NONE', *, *, #4438, .F. ) ;
#2518 = CARTESIAN_POINT ( 'NONE',  ( 3.386276725104728769, 100.0000000000000142, -24.01678749451497907 ) ) ;
#2519 = DIRECTION ( 'NONE',  ( 0.000000000000000000, -1.000000000000000000, 0.000000000000000000 ) ) ;
#2520 = B_SPLINE_SURFACE_WITH_KNOTS ( 'NONE', 3, 1, ( 
 ( #4886, #8864 ),
 ( #1690, #6357 ),
 ( #910, #3314 ),
 ( #370, #1002 ),
 ( #218, #4295 ),
 ( #1101, #5818 ),
 ( #4399, #7479 ),
 ( #7584, #9161 ),
 ( #6646, #2623 ),
 ( #268, #8174 ),
 ( #5176, #2779 ),
 ( #3403, #1878 ),
 ( #4975, #7380 ),
 ( #4195, #3458 ),
 ( #9839, #6597 ),
 ( #1929, #5864 ),
 ( #8220, #9888 ),
 ( #9787, #2672 ),
 ( #9008, #1828 ) ),
 .UNSPECIFIED., .F., .F., .F.,
 ( 4, 1, 1, 1, 1, 1, 1, 1, 1, 1, 1, 1, 1, 1, 1, 1, 4 ),
 ( 2, 2 ),
 ( 0.000000000000000000, 0.06358429906668214282, 0.1250797439647324816, 0.1854075229911844314, 0.2454523280917267347, 0.3052969617611028252, 0.3655926515411210831, 0.4275661794825392770, 0.4916205250740160460, 0.5555554127340263104, 0.6185525978810689773, 0.6803322039413655098, 0.7423868736098769849, 0.8044290668430417179, 0.8676072479036442964, 0.9329923078238739897, 1.000000000000000000 ),
 ( 0.000000000000000000, 1.000000000000000000 ),
 .UNSPECIFIED. ) ;
#2521 = DIRECTION ( 'NONE',  ( 0.000000000000000000, 0.000000000000000000, -1.000000000000000000 ) ) ;
#2522 = CARTESIAN_POINT ( 'NONE',  ( -1.595409442497313560E-16, -4.753124999385482496, -2.605501347177161087 ) ) ;
#2523 = CARTESIAN_POINT ( 'NONE',  ( 0.6698729810778050187, -2.567403810567665090, 2.500000000000000444 ) ) ;
#2524 = CARTESIAN_POINT ( 'NONE',  ( 4.786228327491941173E-16, -4.528124999385482852, 2.605501347177161087 ) ) ;
#2525 = FILL_AREA_STYLE ('',( #8312 ) ) ;
#2526 = CARTESIAN_POINT ( 'NONE',  ( -16.12311789350856017, 99.50000000000000000, 14.86696503675854686 ) ) ;
#2527 = B_SPLINE_CURVE_WITH_KNOTS ( 'NONE', 3,
 ( #4636, #6873, #605, #3745, #7660, #7829, #3902, #10014, #10188, #9223, #9282 ),
 .UNSPECIFIED., .F., .F.,
 ( 4, 1, 1, 1, 1, 1, 1, 1, 4 ),
 ( 0.000000000000000000, 0.1307887167449866828, 0.2576322083635017579, 0.3824781763252146916, 0.5056045358258490774, 0.6278910088851102911, 0.7502354365656509483, 0.8735741898580190457, 1.000000000000000000 ),
 .UNSPECIFIED. ) ;
#2528 = CARTESIAN_POINT ( 'NONE',  ( -19.09188309203678457, 3.500000000000000000, -19.09188309203678813 ) ) ;
#2529 = CARTESIAN_POINT ( 'NONE',  ( 2.912748042341355870, 99.49999999999998579, -22.34826719014139940 ) ) ;
#2530 = CARTESIAN_POINT ( 'NONE',  ( 24.93339342948717885, 99.50000000000000000, -1.235376602564102644 ) ) ;
#2531 = CARTESIAN_POINT ( 'NONE',  ( -20.93486371557392545, 99.49999999999998579, -10.61231311368802466 ) ) ;
#2532 = VERTEX_POINT ( 'NONE', #2843 ) ;
#2533 = ORIENTED_EDGE ( 'NONE', *, *, #2005, .F. ) ;
#2534 = CARTESIAN_POINT ( 'NONE',  ( 11.36312591709336139, 4.399999998907524912, -27.43301270000000258 ) ) ;
#2535 = CARTESIAN_POINT ( 'NONE',  ( 2.971063225226878046, 100.0000000000000000, -23.91837856253154015 ) ) ;
#2536 = CARTESIAN_POINT ( 'NONE',  ( -21.71039561923405969, 100.0000000000000426, -11.44438725057713313 ) ) ;
#2537 = CARTESIAN_POINT ( 'NONE',  ( -2.256430356249998770, -3.365624999385482763, 1.302750673588581876 ) ) ;
#2538 = CARTESIAN_POINT ( 'NONE',  ( -15.07178375341841381, 100.0000000000000000, 16.66969090848992607 ) ) ;
#2539 = CARTESIAN_POINT ( 'NONE',  ( 27.00000000000000355, 1.600000000000000089, 0.000000000000000000 ) ) ;
#2540 = CARTESIAN_POINT ( 'NONE',  ( 19.09188309203678102, 5.299999997815050712, 19.09188309203678813 ) ) ;
#2541 = ADVANCED_FACE ( 'NONE', ( #9900 ), #1325, .T. ) ;
#2542 = CARTESIAN_POINT ( 'NONE',  ( -1.767625397874844694E-16, -3.656249998770965792, -2.886751345948128655 ) ) ;
#2543 = ORIENTED_EDGE ( 'NONE', *, *, #5103, .F. ) ;
#2544 = LINE ( 'NONE', #8925, #5645 ) ;
#2545 = CARTESIAN_POINT ( 'NONE',  ( 0.000000000000000000, -15.00000000000000000, -3.464101615137755275 ) ) ;
#2546 = CARTESIAN_POINT ( 'NONE',  ( 9.357053078540884528, 99.50000000000001421, 19.70216357796830664 ) ) ;
#2547 = CARTESIAN_POINT ( 'NONE',  ( -2.256430356249999214, -4.603124999385482141, 1.302750673588581876 ) ) ;
#2548 = CIRCLE ( 'NONE', #9882, 18.00000000000000000 ) ;
#2549 = ORIENTED_EDGE ( 'NONE', *, *, #914, .F. ) ;
#2550 = ORIENTED_EDGE ( 'NONE', *, *, #4727, .F. ) ;
#2551 = EDGE_CURVE ( 'NONE', #2327, #7711, #6866, .T. ) ;
#2552 = CARTESIAN_POINT ( 'NONE',  ( 8.467217662126737210, 99.50000000000001421, 20.02246181083229004 ) ) ;
#2553 = DIRECTION ( 'NONE',  ( -0.8660254037844385966, 0.000000000000000000, -0.5000000000000001110 ) ) ;
#2554 = CARTESIAN_POINT ( 'NONE',  ( 0.6698729810778112359, -3.676346188203299725, -2.499999999999996447 ) ) ;
#2555 = CARTESIAN_POINT ( 'NONE',  ( 8.540544597724410991, 100.0000000000000000, 19.98924338346217766 ) ) ;
#2556 = EDGE_CURVE ( 'NONE', #3561, #8603, #7905, .T. ) ;
#2557 = CARTESIAN_POINT ( 'NONE',  ( 3.411785164761435674, 100.0000000000000000, -22.76693382491622231 ) ) ;
#2558 = CARTESIAN_POINT ( 'NONE',  ( -0.6698729810778054627, -4.407596189432333667, 2.500000000000000000 ) ) ;
#2559 = CARTESIAN_POINT ( 'NONE',  ( 7.726884419709978857, 99.50000000000000000, 20.74516479202295471 ) ) ;
#2560 = CARTESIAN_POINT ( 'NONE',  ( 3.873456569393397331, 99.50000000000002842, -22.53291374702356364 ) ) ;
#2561 = CARTESIAN_POINT ( 'NONE',  ( 26.99999999999999645, 1.349999997815050312, 11.18376618407358691 ) ) ;
#2562 = DIRECTION ( 'NONE',  ( -1.000000000000000000, 0.000000000000000000, 0.000000000000000000 ) ) ;
#2563 = STYLED_ITEM ( 'NONE', ( #2628 ), #1259 ) ;
#2564 = CARTESIAN_POINT ( 'NONE',  ( -21.59424432678268957, 99.99999999999997158, -9.639623801236600897 ) ) ;
#2565 = CARTESIAN_POINT ( 'NONE',  ( 4.996790860652426159E-15, -1.462499999999999911, -2.500000000000000000 ) ) ;
#2566 = FACE_OUTER_BOUND ( 'NONE', #6252, .T. ) ;
#2567 = VERTEX_POINT ( 'NONE', #2684 ) ;
#2568 = CARTESIAN_POINT ( 'NONE',  ( 2.256430356250000102, -3.965624999385482408, -2.763330213280484622E-16 ) ) ;
#2569 = CARTESIAN_POINT ( 'NONE',  ( -14.79004890936967875, 99.99999999999997158, 16.19006955939758541 ) ) ;
#2570 = CARTESIAN_POINT ( 'NONE',  ( 2.983739933759421259, 99.99999999999998579, -23.28421226151478152 ) ) ;
#2571 = CARTESIAN_POINT ( 'NONE',  ( 11.18376618407357626, 4.650000000000001243, 27.00000000000000000 ) ) ;
#2572 = CARTESIAN_POINT ( 'NONE',  ( 3.195700652717397894, 99.49999999999997158, -22.66286045753255962 ) ) ;
#2573 = EDGE_CURVE ( 'NONE', #6063, #5137, #3517, .T. ) ;
#2574 = CARTESIAN_POINT ( 'NONE',  ( 0.000000000000000000, 0.000000000000000000, 0.000000000000000000 ) ) ;
#2575 = DIRECTION ( 'NONE',  ( 0.000000000000000000, 0.000000000000000000, -1.000000000000000000 ) ) ;
#2576 = CARTESIAN_POINT ( 'NONE',  ( -20.93575003794465061, 99.99999999999998579, -10.12220034237898503 ) ) ;
#2577 = ORIENTED_EDGE ( 'NONE', *, *, #9187, .T. ) ;
#2578 = CARTESIAN_POINT ( 'NONE',  ( 8.132491713109025966, 99.50000000000000000, 21.08089001807756091 ) ) ;
#2579 = CARTESIAN_POINT ( 'NONE',  ( 0.6698729810778063509, -1.426346188203299947, -2.500000000000000000 ) ) ;
#2580 = CARTESIAN_POINT ( 'NONE',  ( -15.43596444985078975, 99.50000000000002842, 15.30036492734783593 ) ) ;
#2581 = CARTESIAN_POINT ( 'NONE',  ( 2.256430356250000102, -2.728124999385482585, -2.763330213280484622E-16 ) ) ;
#2582 = CARTESIAN_POINT ( 'NONE',  ( -22.57971655928959365, 99.50000000000000000, -10.84768434062017839 ) ) ;
#2583 = B_SPLINE_CURVE_WITH_KNOTS ( 'NONE', 1,
 ( #10189, #9510 ),
 .UNSPECIFIED., .F., .F.,
 ( 2, 2 ),
 ( 0.000000000000000000, 1.000000000000000000 ),
 .UNSPECIFIED. ) ;
#2584 = CARTESIAN_POINT ( 'NONE',  ( -22.63784607493503387, 100.0000000000000142, -10.71517552924587058 ) ) ;
#2585 = CARTESIAN_POINT ( 'NONE',  ( 8.337740814200648387, 100.0000000000000284, 20.10843643765939248 ) ) ;
#2586 = CARTESIAN_POINT ( 'NONE',  ( -2.500000000000000000, -5.343749998770965348, 0.000000000000000000 ) ) ;
#2587 = ORIENTED_EDGE ( 'NONE', *, *, #8719, .T. ) ;
#2588 = VERTEX_POINT ( 'NONE', #5189 ) ;
#2589 = CARTESIAN_POINT ( 'NONE',  ( 0.000000000000000000, -25.00000000000000000, 0.000000000000000000 ) ) ;
#2590 = CARTESIAN_POINT ( 'NONE',  ( 3.207057600658871355, 99.99999999999997158, -22.07913334414698880 ) ) ;
#2591 = VECTOR ( 'NONE', #5417, 1000.000000000000000 ) ;
#2592 = ADVANCED_FACE ( 'NONE', ( #5240 ), #10200, .T. ) ;
#2593 = LINE ( 'NONE', #5782, #9716 ) ;
#2594 = CARTESIAN_POINT ( 'NONE',  ( 4.503533123526070270, 99.99999999999998579, -24.63026223303895890 ) ) ;
#2595 = APPLICATION_CONTEXT ( 'automotive_design' ) ;
#2596 = TOROIDAL_SURFACE ( 'NONE', #5935, 23.82500000000000284, 1.324999999999999956 ) ;
#2597 = DIRECTION ( 'NONE',  ( 0.000000000000000000, 0.000000000000000000, 1.000000000000000000 ) ) ;
#2598 = LINE ( 'NONE', #4905, #5671 ) ;
#2599 = CARTESIAN_POINT ( 'NONE',  ( 1.679787559701184688E-15, 5.324999998907524734, -27.43301270000000258 ) ) ;
#2600 = VERTEX_POINT ( 'NONE', #701 ) ;
#2601 = SURFACE_STYLE_USAGE ( .BOTH. , #3871 ) ;
#2602 = ADVANCED_FACE ( 'NONE', ( #9334 ), #7858, .T. ) ;
#2603 = CARTESIAN_POINT ( 'NONE',  ( -1.250000000000000222, -4.574999999999999289, -2.165063509461096825 ) ) ;
#2604 = CARTESIAN_POINT ( 'NONE',  ( 8.429066232339796017, 99.99999999999994316, 19.67794530653910101 ) ) ;
#2605 = ORIENTED_EDGE ( 'NONE', *, *, #5916, .T. ) ;
#2606 = CARTESIAN_POINT ( 'NONE',  ( 9.676361905416721143, 99.50000000000001421, 21.63547735782115566 ) ) ;
#2607 = CARTESIAN_POINT ( 'NONE',  ( 11.18376618407357626, 2.849999997815050978, 27.00000000000000000 ) ) ;
#2608 = DIRECTION ( 'NONE',  ( -0.4980973490458728836, -0.08715574274765840179, -0.8627299156628209786 ) ) ;
#2609 = CARTESIAN_POINT ( 'NONE',  ( -21.87421819196487505, 99.50000000000000000, -9.684578881761979119 ) ) ;
#2610 = CARTESIAN_POINT ( 'NONE',  ( -20.96643530928959365, 99.50000000000000000, -10.05541671241504886 ) ) ;
#2611 = CARTESIAN_POINT ( 'NONE',  ( -22.05902956123343017, 100.0000000000000000, -10.96257574645357558 ) ) ;
#2612 = CARTESIAN_POINT ( 'NONE',  ( 1.250000000000001110, -4.799999999999999822, 2.165063509461096380 ) ) ;
#2613 = CARTESIAN_POINT ( 'NONE',  ( -2.500000000000000000, 0.000000000000000000, 0.000000000000000000 ) ) ;
#2614 = CARTESIAN_POINT ( 'NONE',  ( 0.000000000000000000, 0.000000000000000000, 0.000000000000000000 ) ) ;
#2615 = CARTESIAN_POINT ( 'NONE',  ( 2.958578797724396026, 100.0000000000000000, -23.36432507653281121 ) ) ;
#2616 = CARTESIAN_POINT ( 'NONE',  ( 11.36312591709336139, 1.199999998907525178, -27.43301270000000258 ) ) ;
#2617 = CARTESIAN_POINT ( 'NONE',  ( 1.250000000000001110, -0.6937499987709658811, 2.165063509461096380 ) ) ;
#2618 = CARTESIAN_POINT ( 'NONE',  ( -20.72805389903318130, 100.0000000000000000, -9.848585782927868237 ) ) ;
#2619 = AXIS2_PLACEMENT_3D ( 'NONE', #9645, #8259, #7412 ) ;
#2620 = CARTESIAN_POINT ( 'NONE',  ( 0.000000000000000000, 0.000000000000000000, -2.500000000000000000 ) ) ;
#2621 = CARTESIAN_POINT ( 'NONE',  ( -20.89169796687544789, 99.99999999999998579, -10.40078880447404330 ) ) ;
#2622 = EDGE_LOOP ( 'NONE', ( #10141, #5373, #5393, #1166 ) ) ;
#2623 = CARTESIAN_POINT ( 'NONE',  ( -21.20585021321354802, 99.99999999999998579, -9.381045134209834657 ) ) ;
#2624 = EDGE_CURVE ( 'NONE', #9728, #5955, #2881, .T. ) ;
#2625 = CARTESIAN_POINT ( 'NONE',  ( 3.293272160652527258, 99.99999999999997158, -24.41359064397622802 ) ) ;
#2626 = CARTESIAN_POINT ( 'NONE',  ( 9.575551604960836016, 99.50000000000001421, 20.57049984249936969 ) ) ;
#2627 = ADVANCED_FACE ( 'NONE', ( #3844 ), #1504, .T. ) ;
#2628 = PRESENTATION_STYLE_ASSIGNMENT (( #7532 ) ) ;
#2629 = DIRECTION ( 'NONE',  ( -1.000000000000000000, 0.000000000000000000, 0.000000000000000000 ) ) ;
#2630 = AXIS2_PLACEMENT_3D ( 'NONE', #8118, #5115, #4186 ) ;
#2631 = CARTESIAN_POINT ( 'NONE',  ( 9.877377282685029372E-16, -2.081249998770965615, 2.500000000000000000 ) ) ;
#2632 = CARTESIAN_POINT ( 'NONE',  ( -22.21668755910108928, 99.50000000000004263, -9.472979539922778969 ) ) ;
#2633 = CARTESIAN_POINT ( 'NONE',  ( 0.000000000000000000, 100.0000000000000000, 0.000000000000000000 ) ) ;
#2634 = CARTESIAN_POINT ( 'NONE',  ( -2.499999999999999556, -4.856249998770964638, 1.443375672974065882 ) ) ;
#2635 = ORIENTED_EDGE ( 'NONE', *, *, #4929, .F. ) ;
#2636 = ORIENTED_EDGE ( 'NONE', *, *, #2261, .F. ) ;
#2637 = AXIS2_PLACEMENT_3D ( 'NONE', #9316, #4499, #2032 ) ;
#2638 = CARTESIAN_POINT ( 'NONE',  ( -21.20999280589743918, 100.0000000000000284, -11.35389291771566000 ) ) ;
#2639 = CARTESIAN_POINT ( 'NONE',  ( 3.317038232150706367, 99.99999999999995737, -21.66195598387956878 ) ) ;
#2640 = LINE ( 'NONE', #6661, #10056 ) ;
#2641 = CARTESIAN_POINT ( 'NONE',  ( -15.11748654497029953, 99.99999999999998579, 15.76872032455190897 ) ) ;
#2642 = CIRCLE ( 'NONE', #8500, 2.062556682370379590 ) ;
#2643 = CARTESIAN_POINT ( 'NONE',  ( 8.149445629999579666, 99.50000000000002842, 20.33980848884064230 ) ) ;
#2644 =( BOUNDED_CURVE ( )  B_SPLINE_CURVE ( 2, ( #388, #1171, #4570, #9912, #3843, #10231, #596, #6768, #8342 ),
 .UNSPECIFIED., .F., .F. ) 
 B_SPLINE_CURVE_WITH_KNOTS ( ( 3, 2, 2, 2, 3 ),
 ( 0.4642857142857143016, 0.4821428571428571508, 0.5000000000000000000, 0.5178571428571429047, 0.5357142857142856984 ),
 .UNSPECIFIED. ) 
 CURVE ( )  GEOMETRIC_REPRESENTATION_ITEM ( )  RATIONAL_B_SPLINE_CURVE ( ( 1.000000000000000000, 0.9238795325112867385, 1.000000000000000000, 0.9238795325112867385, 1.000000000000000000, 0.9238795325112867385, 1.000000000000000000, 0.9238795325112867385, 1.000000000000000000 ) ) 
 REPRESENTATION_ITEM ( '' )  );
#2645 = CARTESIAN_POINT ( 'NONE',  ( 9.248677610544923766, 100.0000000000000000, 22.83089001807756446 ) ) ;
#2646 = CARTESIAN_POINT ( 'NONE',  ( -21.37606745505193473, 100.0000000000000284, -11.05925878703054011 ) ) ;
#2647 = VERTEX_POINT ( 'NONE', #7376 ) ;
#2648 = CARTESIAN_POINT ( 'NONE',  ( 3.058419780146050648, 100.0000000000000000, -23.12871267107006545 ) ) ;
#2649 = CARTESIAN_POINT ( 'NONE',  ( -5.039362679103552881E-15, 4.849999998907525089, 27.43301270000000258 ) ) ;
#2650 = CARTESIAN_POINT ( 'NONE',  ( -2.499999999999999112, -2.156249998770965348, 1.443375672974065882 ) ) ;
#2651 = CARTESIAN_POINT ( 'NONE',  ( -20.42657152723830905, 99.99999999999997158, -10.54129411626120216 ) ) ;
#2652 = CARTESIAN_POINT ( 'NONE',  ( 7.746148141271532950, 99.50000000000002842, 20.51930889200067298 ) ) ;
#2653 = CARTESIAN_POINT ( 'NONE',  ( 3.477525819554967423, 100.0000000000000284, -22.44236894434852658 ) ) ;
#2654 = CARTESIAN_POINT ( 'NONE',  ( 19.09188309203678813, 4.699999997815051067, -19.09188309203678813 ) ) ;
#2655 = CARTESIAN_POINT ( 'NONE',  ( -20.42657152723830905, 99.50000000000000000, -10.54129411626120216 ) ) ;
#2656 = CARTESIAN_POINT ( 'NONE',  ( -21.80427673524616239, 99.50000000000000000, -9.663674634844889866 ) ) ;
#2657 = CARTESIAN_POINT ( 'NONE',  ( 3.891852272358404807, 100.0000000000000142, -22.89765557720719968 ) ) ;
#2658 = EDGE_CURVE ( 'NONE', #7769, #8491, #7787, .T. ) ;
#2659 = PLANE ( 'NONE',  #7265 ) ;
#2660 = CARTESIAN_POINT ( 'NONE',  ( 4.750280232731688201, 99.50000000000002842, -24.05275076595185624 ) ) ;
#2661 = ORIENTED_EDGE ( 'NONE', *, *, #6569, .T. ) ;
#2662 = CARTESIAN_POINT ( 'NONE',  ( 1.128215178124999607, -3.440624999385482496, -1.954126010382871259 ) ) ;
#2663 = CARTESIAN_POINT ( 'NONE',  ( -14.97579057656165169, 100.0000000000000000, 16.56690896377573452 ) ) ;
#2664 = CARTESIAN_POINT ( 'NONE',  ( 2.927917759182871560, 99.99999999999997158, -23.69257214368879261 ) ) ;
#2665 = CARTESIAN_POINT ( 'NONE',  ( 11.36312591709336850, 2.499999998907525445, 27.43301269999999903 ) ) ;
#2666 = CARTESIAN_POINT ( 'NONE',  ( 0.6698729810778063509, -0.5263461882032999251, -2.500000000000000000 ) ) ;
#2667 = DIRECTION ( 'NONE',  ( 0.000000000000000000, 0.000000000000000000, 1.000000000000000000 ) ) ;
#2668 = DIRECTION ( 'NONE',  ( 0.000000000000000000, -1.000000000000000000, 0.000000000000000000 ) ) ;
#2669 = FILL_AREA_STYLE_COLOUR ( '', #5576 ) ;
#2670 = EDGE_CURVE ( 'NONE', #3656, #1838, #955, .T. ) ;
#2671 = ORIENTED_EDGE ( 'NONE', *, *, #1918, .F. ) ;
#2672 = CARTESIAN_POINT ( 'NONE',  ( -22.05573893622344173, 99.99999999999994316, -9.391591294897233766 ) ) ;
#2673 = CARTESIAN_POINT ( 'NONE',  ( -11.36312591709335962, 4.499999998907525445, -27.43301270000000258 ) ) ;
#2674 = CARTESIAN_POINT ( 'NONE',  ( -16.34436021381890924, 99.50000000000000000, 15.38072013554846151 ) ) ;
#2675 =( NAMED_UNIT ( * ) PLANE_ANGLE_UNIT ( ) SI_UNIT ( $, .RADIAN. ) );
#2676 = EDGE_CURVE ( 'NONE', #4679, #7989, #7284, .T. ) ;
#2677 = CARTESIAN_POINT ( 'NONE',  ( 4.996790860652426159E-15, -1.856249998770965748, -2.500000000000000000 ) ) ;
#2678 = CARTESIAN_POINT ( 'NONE',  ( 8.564701892180647036, 99.50000000000000000, 19.97971282122689018 ) ) ;
#2679 = CARTESIAN_POINT ( 'NONE',  ( 3.563396934924631942, 99.50000000000001421, -22.47881610735839431 ) ) ;
#2680 = PRODUCT_DEFINITION ( 'UNKNOWN', '', #631, #5281 ) ;
#2681 = CARTESIAN_POINT ( 'NONE',  ( -21.08523985030068459, 100.0000000000000000, -9.874866134143449159 ) ) ;
#2682 = VERTEX_POINT ( 'NONE', #4099 ) ;
#2683 = EDGE_CURVE ( 'NONE', #6501, #2239, #3400, .T. ) ;
#2684 = CARTESIAN_POINT ( 'NONE',  ( 7.156925775808251622, 99.50000000000000000, 23.91622092442889524 ) ) ;
#2685 = EDGE_CURVE ( 'NONE', #6993, #2880, #7232, .T. ) ;
#2686 = CARTESIAN_POINT ( 'NONE',  ( -2.500000000000000000, -3.993749998770965703, 0.000000000000000000 ) ) ;
#2687 = EDGE_LOOP ( 'NONE', ( #6131, #6118, #754, #8186 ) ) ;
#2688 = DIRECTION ( 'NONE',  ( 0.000000000000000000, 0.000000000000000000, 1.000000000000000000 ) ) ;
#2689 = CARTESIAN_POINT ( 'NONE',  ( 3.283294465904739390, 100.0000000000000000, -21.71066637097430885 ) ) ;
#2690 = ADVANCED_FACE ( 'NONE', ( #124 ), #3263, .T. ) ;
#2691 = CARTESIAN_POINT ( 'NONE',  ( 9.184850993605147944E-16, 87.00000000000001421, 7.500000000000000000 ) ) ;
#2692 = CARTESIAN_POINT ( 'NONE',  ( -2.500000000000000000, -0.3937499987709658922, 0.000000000000000000 ) ) ;
#2693 = EDGE_LOOP ( 'NONE', ( #5365, #6331, #9868, #9244 ) ) ;
#2694 = CARTESIAN_POINT ( 'NONE',  ( 8.281567445270807681, 99.50000000000000000, 20.15885744430370252 ) ) ;
#2695 = EDGE_CURVE ( 'NONE', #7425, #3613, #3069, .T. ) ;
#2696 = DIRECTION ( 'NONE',  ( -0.000000000000000000, 1.000000000000000000, -0.000000000000000000 ) ) ;
#2697 = CARTESIAN_POINT ( 'NONE',  ( -21.30928386698190025, 100.0000000000000000, -11.02857376369709996 ) ) ;
#2698 = DIRECTION ( 'NONE',  ( 0.000000000000000000, 1.000000000000000000, 0.000000000000000000 ) ) ;
#2699 = ORIENTED_EDGE ( 'NONE', *, *, #7028, .T. ) ;
#2700 = CARTESIAN_POINT ( 'NONE',  ( -4.959819536546781389E-15, 1.199999997815050401, 27.00000000000000355 ) ) ;
#2701 = CARTESIAN_POINT ( 'NONE',  ( -19.39806930854668465, 3.249999998907525001, 19.39806930854667755 ) ) ;
#2702 = CARTESIAN_POINT ( 'NONE',  ( 0.000000000000000000, 72.50000000000001421, 0.000000000000000000 ) ) ;
#2703 = CARTESIAN_POINT ( 'NONE',  ( 4.061354557346970040, 99.99999999999994316, -22.84864678426182039 ) ) ;
#2704 = CARTESIAN_POINT ( 'NONE',  ( 3.949943451936506644, 99.99999999999997158, -21.41482314084395711 ) ) ;
#2705 = CARTESIAN_POINT ( 'NONE',  ( -20.74358258379034936, 99.99999999999998579, -9.818556592845180120 ) ) ;
#2706 = CARTESIAN_POINT ( 'NONE',  ( 27.00000000000000355, 5.399999997815051245, 0.000000000000000000 ) ) ;
#2707 =( BOUNDED_SURFACE ( )  B_SPLINE_SURFACE ( 1, 2, ( 
 ( #607, #7718, #1998, #5197, #7775, #3805, #5937, #2745, #3641, #2852, #1951, #9131, #5146, #6037, #2059, #554, #6932, #3131, #7094, #2391, #10351, #3855, #2287, #3908, #3077, #5587, #9607, #7832, #8825, #822, #2439, #3181, #7881, #5634, #7042, #9460, #8773, #4639, #5433, #1654, #8727, #4845, #1551, #8675, #25, #3028, #4741, #713, #6366, #3229, #5536, #8622, #8038, #661, #1600, #10246, #4693, #2230, #871, #4790, #4062, #6319, #1498, #10297, #1446, #9512, #2336, #6261, #7988, #6204, #5485, #769, #10193, #9403, #7936, #3960, #4013, #7147, #9560, #7197, #6417, #9019, #8282, #1012, #8138, #9848, #178, #2542, #9073, #1789, #3324, #8875, #5875, #9658, #4985, #7344, #2686, #1887, #8091, #9750, #7246, #7388, #6513, #1698, #5081, #6606, #135, #4896, #6657, #1113, #83, #3278, #4113, #921, #6467, #2493, #4255, #8923, #5686, #2634, #7298, #3365, #4160, #9798, #228, #9702, #5734, #968, #1742, #5827, #4939, #6560, #2586, #8231, #5778 ),
 ( #8972, #1836, #8184, #4204, #3411, #1062, #5032, #7435, #3470, #276, #329, #4356, #1165, #7710, #2165, #5242, #10121, #2050, #381, #3632, #1219, #4304, #7540, #1941, #3739, #6921, #7490, #2958, #3574, #5136, #3518, #6139, #1326, #5979, #9336, #10063, #5366, #7595, #4411, #6867, #4462, #8335, #6759, #8388, #9957, #2900, #8555, #2791, #6705, #5302, #9902, #7652, #1991, #2737, #489, #433, #5923, #4515, #6812, #3683, #6084, #2844, #8441, #10009, #9275, #9172, #5190, #6029, #545, #2106, #8498, #9121, #9218, #1271, #9391, #3122, #2220, #7871, #8612, #652, #3949, #6194, #6980, #7187, #10288, #6404, #6307, #10234, #1588, #4573, #9503, #9449, #4731, #4780, #7084, #10181, #3218, #5424, #7135, #1437, #6250, #3795, #4003, #10340, #16, #4684, #3066, #2278, #3017, #703, #5474, #4630, #3172, #7768, #7822, #2328, #5624, #9596, #3846, #2427, #6356, #8666, #3896, #599, #9550, #2377, #1381, #5525, #1489, #7031, #8717, #1535, #7925, #757, #5574 ) ),
 .UNSPECIFIED., .F., .F., .F. ) 
 B_SPLINE_SURFACE_WITH_KNOTS ( ( 2, 2 ),
 ( 3, 2, 2, 2, 2, 2, 2, 2, 2, 2, 2, 2, 2, 2, 2, 2, 2, 2, 2, 2, 2, 2, 2, 2, 2, 2, 2, 2, 2, 2, 2, 2, 2, 2, 2, 2, 2, 2, 2, 2, 2, 2, 2, 2, 2, 2, 2, 2, 2, 2, 2, 2, 2, 2, 2, 2, 2, 2, 2, 2, 2, 2, 2, 2, 2, 2, 2, 3 ),
 ( 0.000000000000000000, 1.000000000000000000 ),
 ( 0.000000000000000000, 0.01388888888888888812, 0.02777777777777777624, 0.04166666666666666435, 0.05555555555555555247, 0.06944444444444444753, 0.08333333333333332871, 0.09722222222222222376, 0.1111111111111111049, 0.1250000000000000000, 0.1388888888888888951, 0.1527777777777777901, 0.1666666666666666574, 0.1805555555555555525, 0.1944444444444444475, 0.2083333333333333426, 0.2222222222222222099, 0.2361111111111111049, 0.2500000000000000000, 0.2638888888888888951, 0.2777777777777777901, 0.2916666666666666852, 0.3055555555555555802, 0.3194444444444444198, 0.3333333333333333148, 0.3472222222222222099, 0.3611111111111111049, 0.3750000000000000000, 0.3888888888888888951, 0.4027777777777777901, 0.4166666666666666852, 0.4305555555555555802, 0.4444444444444444198, 0.4583333333333333148, 0.4722222222222222099, 0.4861111111111111049, 0.5000000000000000000, 0.5138888888888888395, 0.5277777777777777901, 0.5416666666666666297, 0.5555555555555555802, 0.5694444444444444198, 0.5833333333333333703, 0.5972222222222222099, 0.6111111111111111605, 0.6250000000000000000, 0.6388888888888888395, 0.6527777777777777901, 0.6666666666666666297, 0.6805555555555555802, 0.6944444444444444198, 0.7083333333333333703, 0.7222222222222222099, 0.7361111111111111605, 0.7500000000000000000, 0.7638888888888888395, 0.7777777777777777901, 0.7916666666666666297, 0.8055555555555555802, 0.8194444444444444198, 0.8333333333333333703, 0.8472222222222222099, 0.8611111111111111605, 0.8750000000000000000, 0.8888888888888888395, 0.9027777777777777901, 0.9166666666666666297, 0.9258784959437954543 ),
 .UNSPECIFIED. ) 
 GEOMETRIC_REPRESENTATION_ITEM ( )  RATIONAL_B_SPLINE_SURFACE ( (
 ( 1.000000000000000000, 0.8660254037844387076, 1.000000000000000000, 0.8660254037844387076, 1.000000000000000000, 0.8660254037844387076, 1.000000000000000000, 0.8660254037844387076, 1.000000000000000000, 0.8660254037844387076, 1.000000000000000000, 0.8660254037844387076, 1.000000000000000000, 0.8660254037844387076, 1.000000000000000000, 0.8660254037844387076, 1.000000000000000000, 0.8660254037844387076, 1.000000000000000000, 0.8660254037844387076, 1.000000000000000000, 0.8660254037844387076, 1.000000000000000000, 0.8660254037844387076, 1.000000000000000000, 0.8660254037844387076, 1.000000000000000000, 0.8660254037844387076, 1.000000000000000000, 0.8660254037844387076, 1.000000000000000000, 0.8660254037844387076, 1.000000000000000000, 0.8660254037844387076, 1.000000000000000000, 0.8660254037844387076, 1.000000000000000000, 0.8660254037844387076, 1.000000000000000000, 0.8660254037844387076, 1.000000000000000000, 0.8660254037844387076, 1.000000000000000000, 0.8660254037844387076, 1.000000000000000000, 0.8660254037844387076, 1.000000000000000000, 0.8660254037844387076, 1.000000000000000000, 0.8660254037844387076, 1.000000000000000000, 0.8660254037844387076, 1.000000000000000000, 0.8660254037844387076, 1.000000000000000000, 0.8660254037844387076, 1.000000000000000000, 0.8660254037844387076, 1.000000000000000000, 0.8660254037844387076, 1.000000000000000000, 0.8660254037844387076, 1.000000000000000000, 0.8660254037844387076, 1.000000000000000000, 0.8660254037844387076, 1.000000000000000000, 0.8660254037844387076, 1.000000000000000000, 0.8660254037844387076, 1.000000000000000000, 0.8660254037844387076, 1.000000000000000000, 0.8660254037844387076, 1.000000000000000000, 0.8660254037844387076, 1.000000000000000000, 0.8660254037844387076, 1.000000000000000000, 0.8660254037844387076, 1.000000000000000000, 0.8660254037844387076, 1.000000000000000000, 0.8660254037844387076, 1.000000000000000000, 0.8660254037844387076, 1.000000000000000000, 0.8660254037844387076, 1.000000000000000000, 0.8660254037844387076, 1.000000000000000000, 0.8660254037844387076, 1.000000000000000000, 0.8660254037844387076, 1.000000000000000000, 0.8660254037844387076, 1.000000000000000000, 0.8660254037844387076, 1.000000000000000000, 0.8660254037844387076, 1.000000000000000000, 0.8660254037844387076, 1.000000000000000000, 0.8660254037844387076, 1.000000000000000000, 0.8660254037844387076, 1.000000000000000000, 0.8660254037844387076, 1.000000000000000000, 0.8660254037844387076, 1.000000000000000000, 0.8660254037844387076, 1.000000000000000000, 0.8660254037844387076, 1.000000000000000000, 0.8660254037844387076, 1.000000000000000000, 0.8660254037844387076, 1.000000000000000000, 0.8660254037844387076, 1.000000000000000000, 0.8660254037844387076, 1.000000000000000000, 0.8660254037844387076, 1.000000000000000000, 0.8660254037844387076, 1.000000000000000000, 0.8660254037844387076, 1.000000000000000000, 0.8660254037844387076, 1.000000000000000000, 0.8660254037844387076, 1.000000000000000000, 0.9111411202376789031, 0.9401538480137057174),
 ( 1.000000000000000000, 0.8660254037844387076, 1.000000000000000000, 0.8660254037844387076, 1.000000000000000000, 0.8660254037844387076, 1.000000000000000000, 0.8660254037844387076, 1.000000000000000000, 0.8660254037844387076, 1.000000000000000000, 0.8660254037844387076, 1.000000000000000000, 0.8660254037844387076, 1.000000000000000000, 0.8660254037844387076, 1.000000000000000000, 0.8660254037844387076, 1.000000000000000000, 0.8660254037844387076, 1.000000000000000000, 0.8660254037844387076, 1.000000000000000000, 0.8660254037844387076, 1.000000000000000000, 0.8660254037844387076, 1.000000000000000000, 0.8660254037844387076, 1.000000000000000000, 0.8660254037844387076, 1.000000000000000000, 0.8660254037844387076, 1.000000000000000000, 0.8660254037844387076, 1.000000000000000000, 0.8660254037844387076, 1.000000000000000000, 0.8660254037844387076, 1.000000000000000000, 0.8660254037844387076, 1.000000000000000000, 0.8660254037844387076, 1.000000000000000000, 0.8660254037844387076, 1.000000000000000000, 0.8660254037844387076, 1.000000000000000000, 0.8660254037844387076, 1.000000000000000000, 0.8660254037844387076, 1.000000000000000000, 0.8660254037844387076, 1.000000000000000000, 0.8660254037844387076, 1.000000000000000000, 0.8660254037844387076, 1.000000000000000000, 0.8660254037844387076, 1.000000000000000000, 0.8660254037844387076, 1.000000000000000000, 0.8660254037844387076, 1.000000000000000000, 0.8660254037844387076, 1.000000000000000000, 0.8660254037844387076, 1.000000000000000000, 0.8660254037844387076, 1.000000000000000000, 0.8660254037844387076, 1.000000000000000000, 0.8660254037844387076, 1.000000000000000000, 0.8660254037844387076, 1.000000000000000000, 0.8660254037844387076, 1.000000000000000000, 0.8660254037844387076, 1.000000000000000000, 0.8660254037844387076, 1.000000000000000000, 0.8660254037844387076, 1.000000000000000000, 0.8660254037844387076, 1.000000000000000000, 0.8660254037844387076, 1.000000000000000000, 0.8660254037844387076, 1.000000000000000000, 0.8660254037844387076, 1.000000000000000000, 0.8660254037844387076, 1.000000000000000000, 0.8660254037844387076, 1.000000000000000000, 0.8660254037844387076, 1.000000000000000000, 0.8660254037844387076, 1.000000000000000000, 0.8660254037844387076, 1.000000000000000000, 0.8660254037844387076, 1.000000000000000000, 0.8660254037844387076, 1.000000000000000000, 0.8660254037844387076, 1.000000000000000000, 0.8660254037844387076, 1.000000000000000000, 0.8660254037844387076, 1.000000000000000000, 0.8660254037844387076, 1.000000000000000000, 0.8660254037844387076, 1.000000000000000000, 0.8660254037844387076, 1.000000000000000000, 0.8660254037844387076, 1.000000000000000000, 0.8660254037844387076, 1.000000000000000000, 0.8660254037844387076, 1.000000000000000000, 0.8660254037844387076, 1.000000000000000000, 0.8660254037844387076, 1.000000000000000000, 0.8660254037844387076, 1.000000000000000000, 0.8660254037844387076, 1.000000000000000000, 0.8660254037844387076, 1.000000000000000000, 0.9111411202376789031, 0.9401538480137057174) ) ) 
 REPRESENTATION_ITEM ( '' )  SURFACE ( )  );
#2708 = CARTESIAN_POINT ( 'NONE',  ( 3.061616997868383141E-16, 0.000000000000000000, 2.500000000000000000 ) ) ;
#2709 = CARTESIAN_POINT ( 'NONE',  ( -21.08523985030068459, 99.50000000000000000, -9.874866134143449159 ) ) ;
#2710 = CARTESIAN_POINT ( 'NONE',  ( 9.877377282685029372E-16, -0.3374999999999999667, 2.500000000000000000 ) ) ;
#2711 = CARTESIAN_POINT ( 'NONE',  ( -21.33175168474226879, 99.50000000000001421, -11.03889704119913162 ) ) ;
#2712 = FACE_OUTER_BOUND ( 'NONE', #6941, .T. ) ;
#2713 = CARTESIAN_POINT ( 'NONE',  ( -2.256430356249998770, -5.053124999385482319, 1.302750673588581876 ) ) ;
#2714 = ORIENTED_EDGE ( 'NONE', *, *, #8288, .T. ) ;
#2715 = CARTESIAN_POINT ( 'NONE',  ( -2.499999999999999556, -0.8624999999999998224, 1.443375672974065882 ) ) ;
#2716 = CARTESIAN_POINT ( 'NONE',  ( -2.500000000000000000, -2.699999999999999734, 0.000000000000000000 ) ) ;
#2717 = CARTESIAN_POINT ( 'NONE',  ( -1.128215178125000273, -0.3281249993854828961, -1.954126010382871259 ) ) ;
#2718 = CARTESIAN_POINT ( 'NONE',  ( -19.39806930854668465, 1.549999998907525489, 19.39806930854667755 ) ) ;
#2719 = CARTESIAN_POINT ( 'NONE',  ( -2.500000000000000000, -0.9000000000000000222, 0.000000000000000000 ) ) ;
#2720 = PRESENTATION_LAYER_ASSIGNMENT (  '', '', ( #7237 ) ) ;
#2721 = LINE ( 'NONE', #1925, #6603 ) ;
#2722 = CARTESIAN_POINT ( 'NONE',  ( 2.939152317953647500E-15, 70.00000000000000000, -23.99999999999999645 ) ) ;
#2723 = CARTESIAN_POINT ( 'NONE',  ( 0.000000000000000000, 75.00000000000001421, -18.23673019291534558 ) ) ;
#2724 = EDGE_LOOP ( 'NONE', ( #9775, #2480, #2577, #9898 ) ) ;
#2725 = FACE_OUTER_BOUND ( 'NONE', #1660, .T. ) ;
#2726 = CARTESIAN_POINT ( 'NONE',  ( -21.98271324694694329, 99.50000000000000000, -11.39207625356720222 ) ) ;
#2727 = CARTESIAN_POINT ( 'NONE',  ( 10.72103337977569204, 100.0000000000000000, 22.20268488987243316 ) ) ;
#2728 = COLOUR_RGB ( '',0.8941176470588234615, 0.8941176470588234615, 0.8941176470588234615 ) ;
#2729 = CARTESIAN_POINT ( 'NONE',  ( 9.342627931057743140, 99.50000000000000000, 21.59831790269294771 ) ) ;
#2730 = CARTESIAN_POINT ( 'NONE',  ( 4.277141017070624329, 100.0000000000000284, -21.57940364907851816 ) ) ;
#2731 = CARTESIAN_POINT ( 'NONE',  ( 9.446088657802272692, 99.50000000000004263, 20.22669104216016578 ) ) ;
#2732 = ADVANCED_FACE ( 'NONE', ( #2832 ), #3671, .T. ) ;
#2733 = CARTESIAN_POINT ( 'NONE',  ( 3.291601991079349698, 99.49999999999997158, -22.28586332678438353 ) ) ;
#2734 = DIRECTION ( 'NONE',  ( -0.000000000000000000, -1.000000000000000000, -0.000000000000000000 ) ) ;
#2735 = ORIENTED_EDGE ( 'NONE', *, *, #5617, .F. ) ;
#2736 = CARTESIAN_POINT ( 'NONE',  ( -16.11976138926855739, 99.99999999999997158, 16.60078749809536447 ) ) ;
#2737 = CARTESIAN_POINT ( 'NONE',  ( 2.256430356249999658, -2.240624999385482319, -1.302750673588581432 ) ) ;
#2738 = ORIENTED_EDGE ( 'NONE', *, *, #1843, .F. ) ;
#2739 = CARTESIAN_POINT ( 'NONE',  ( -16.36254897777739004, 99.50000000000001421, 15.39785597259249350 ) ) ;
#2740 = CARTESIAN_POINT ( 'NONE',  ( -4.357666448243394824E-15, -2.587499999999999467, 2.500000000000000000 ) ) ;
#2741 = CARTESIAN_POINT ( 'NONE',  ( -22.28244091826395135, 99.50000000000000000, -10.68852969318427881 ) ) ;
#2742 = CARTESIAN_POINT ( 'NONE',  ( -15.30604604128650692, 100.0000000000000000, 15.41317891555018349 ) ) ;
#2743 = ORIENTED_EDGE ( 'NONE', *, *, #4990, .F. ) ;
#2744 = CARTESIAN_POINT ( 'NONE',  ( -16.52157078939288937, 99.49999999999998579, 16.20087177393598665 ) ) ;
#2745 = CARTESIAN_POINT ( 'NONE',  ( 2.500000000000000444, -0.6562499987709659033, 1.443375672974063439 ) ) ;
#2746 = DIRECTION ( 'NONE',  ( 1.000000000000000000, 0.000000000000000000, 6.123233995736763571E-17 ) ) ;
#2747 = LINE ( 'NONE', #3481, #5479 ) ;
#2748 = VERTEX_POINT ( 'NONE', #7582 ) ;
#2749 = B_SPLINE_CURVE_WITH_KNOTS ( 'NONE', 3,
 ( #523, #9844, #8179, #7684, #9306, #2138, #1007, #5339, #8529, #4981, #9746, #4157, #3362, #6555, #2582 ),
 .UNSPECIFIED., .F., .F.,
 ( 4, 1, 1, 1, 1, 1, 1, 1, 1, 1, 1, 1, 4 ),
 ( 0.000000000000000000, 0.08595325681623211533, 0.1695367914770939399, 0.2510169726856145700, 0.3324720360531058239, 0.4139176782331075444, 0.4946662699496591764, 0.5765962148649595997, 0.6610575120797289594, 0.7465372922784411225, 0.8302848992160567487, 0.9144215288650135998, 1.000000000000000000 ),
 .UNSPECIFIED. ) ;
#2750 = EDGE_CURVE ( 'NONE', #8902, #9406, #1210, .T. ) ;
#2751 = DIRECTION ( 'NONE',  ( -0.000000000000000000, 1.000000000000000000, -0.000000000000000000 ) ) ;
#2752 = CARTESIAN_POINT ( 'NONE',  ( -27.43301270000000258, 3.899999998907525356, -11.36312591709336317 ) ) ;
#2753 = LINE ( 'NONE', #397, #4061 ) ;
#2754 = EDGE_CURVE ( 'NONE', #728, #4302, #9837, .T. ) ;
#2755 = CARTESIAN_POINT ( 'NONE',  ( 2.950788281418828429, 99.50000000000001421, -23.82341910423825837 ) ) ;
#2756 = LINE ( 'NONE', #197, #2947 ) ;
#2757 = VECTOR ( 'NONE', #6777, 1000.000000000000000 ) ;
#2758 = ORIENTED_EDGE ( 'NONE', *, *, #9480, .F. ) ;
#2759 = CARTESIAN_POINT ( 'NONE',  ( 0.000000000000000000, -20.00000000000000000, 0.000000000000000000 ) ) ;
#2760 = CARTESIAN_POINT ( 'NONE',  ( -4.959819536546781389E-15, 5.199999997815050179, 27.00000000000000355 ) ) ;
#2761 = ORIENTED_EDGE ( 'NONE', *, *, #6691, .F. ) ;
#2762 = DIRECTION ( 'NONE',  ( 0.000000000000000000, 0.000000000000000000, -1.000000000000000000 ) ) ;
#2763 = CARTESIAN_POINT ( 'NONE',  ( -20.96643530928959720, 99.50000000000001421, -10.05541671241505064 ) ) ;
#2764 = CARTESIAN_POINT ( 'NONE',  ( -2.500000000000000000, -0.4500000000000000111, 0.000000000000000000 ) ) ;
#2765 = VERTEX_POINT ( 'NONE', #2723 ) ;
#2766 = CARTESIAN_POINT ( 'NONE',  ( 4.906732565843439531, 99.50000000000001421, -23.57187248890526376 ) ) ;
#2767 = CARTESIAN_POINT ( 'NONE',  ( 0.000000000000000000, 85.00000000000000000, 0.000000000000000000 ) ) ;
#2768 = CARTESIAN_POINT ( 'NONE',  ( -1.250000000000000222, -0.9749999999999999778, -2.165063509461096825 ) ) ;
#2769 = DIRECTION ( 'NONE',  ( 1.000000000000000000, 0.000000000000000000, 0.000000000000000000 ) ) ;
#2770 = DIRECTION ( 'NONE',  ( 0.000000000000000000, 0.000000000000000000, -1.000000000000000000 ) ) ;
#2771 = VECTOR ( 'NONE', #2841, 1000.000000000000000 ) ;
#2772 = CARTESIAN_POINT ( 'NONE',  ( 2.940192896829773250, 99.50000000000001421, -23.44521981770616037 ) ) ;
#2773 = CARTESIAN_POINT ( 'NONE',  ( 11.36312591709336139, 1.999999998907525223, -27.43301270000000258 ) ) ;
#2774 = CARTESIAN_POINT ( 'NONE',  ( 9.877377282685029372E-16, -0.7312499987709657479, 2.500000000000000000 ) ) ;
#2775 = ORIENTED_EDGE ( 'NONE', *, *, #8873, .F. ) ;
#2776 = CARTESIAN_POINT ( 'NONE',  ( 0.000000000000000000, 100.0000000000000000, 0.000000000000000000 ) ) ;
#2777 = FACE_OUTER_BOUND ( 'NONE', #6425, .T. ) ;
#2778 = CARTESIAN_POINT ( 'NONE',  ( -27.00000000000000355, 4.199999997815050179, -3.306546357697854128E-15 ) ) ;
#2779 = CARTESIAN_POINT ( 'NONE',  ( -21.39817337045129619, 99.99999999999994316, -9.317726141196148504 ) ) ;
#2780 = CARTESIAN_POINT ( 'NONE',  ( 4.835062408351179286, 99.50000000000000000, -21.79588013901878440 ) ) ;
#2781 = CARTESIAN_POINT ( 'NONE',  ( 3.000000000000000000, -15.00000000000000000, 1.732050807568879192 ) ) ;
#2782 = CARTESIAN_POINT ( 'NONE',  ( 9.583828860305853681, 99.49999999999998579, 20.68614437522342797 ) ) ;
#2783 = CARTESIAN_POINT ( 'NONE',  ( 9.513000527211589841, 100.0000000000000000, 20.35102222961602436 ) ) ;
#2784 = CARTESIAN_POINT ( 'NONE',  ( 3.252389375388976323, 99.50000000000004263, -22.22144413113850447 ) ) ;
#2785 = AXIS2_PLACEMENT_3D ( 'NONE', #3634, #7712, #6816 ) ;
#2786 = DIRECTION ( 'NONE',  ( 0.000000000000000000, 0.000000000000000000, -1.000000000000000000 ) ) ;
#2787 = ORIENTED_EDGE ( 'NONE', *, *, #1705, .F. ) ;
#2788 = ORIENTED_EDGE ( 'NONE', *, *, #2224, .F. ) ;
#2789 = CARTESIAN_POINT ( 'NONE',  ( -15.98323291606820362, 99.99999999999998579, 16.64087298452848884 ) ) ;
#2790 = CLOSED_SHELL ( 'NONE', ( #2116, #10132, #5453, #1755, #9213, #7285, #7034, #7008, #6121 ) ) ;
#2791 = CARTESIAN_POINT ( 'NONE',  ( -2.256430356249999214, -2.015624999385482674, 1.302750673588581876 ) ) ;
#2792 = ORIENTED_EDGE ( 'NONE', *, *, #1792, .T. ) ;
#2793 = EDGE_CURVE ( 'NONE', #3366, #224, #2389, .T. ) ;
#2794 = CARTESIAN_POINT ( 'NONE',  ( -22.17094027205346052, 99.50000000000001421, -9.884352203306939089 ) ) ;
#2795 = CARTESIAN_POINT ( 'NONE',  ( -27.43301270000000969, 0.6999999989075252893, 11.36312591709335784 ) ) ;
#2796 = LINE ( 'NONE', #9804, #7216 ) ;
#2797 = CARTESIAN_POINT ( 'NONE',  ( -15.22739782325755442, 99.99999999999998579, 15.50750051783781025 ) ) ;
#2798 = AXIS2_PLACEMENT_3D ( 'NONE', #5730, #9011, #8916 ) ;
#2799 = CARTESIAN_POINT ( 'NONE',  ( 0.000000000000000000, 85.00000000000000000, -25.15000000000000213 ) ) ;
#2800 = ORIENTED_EDGE ( 'NONE', *, *, #6106, .T. ) ;
#2801 = EDGE_CURVE ( 'NONE', #4986, #6736, #4565, .T. ) ;
#2802 = CARTESIAN_POINT ( 'NONE',  ( -3.486133158594716510E-16, -2.756249998770965437, -2.500000000000000000 ) ) ;
#2803 = CARTESIAN_POINT ( 'NONE',  ( 1.249999999999999334, -2.399999999999999911, -2.165063509461096825 ) ) ;
#2804 = VERTEX_POINT ( 'NONE', #5968 ) ;
#2805 = CARTESIAN_POINT ( 'NONE',  ( 26.99999999999999645, 1.349999997815050312, 11.18376618407358691 ) ) ;
#2806 = MANIFOLD_SOLID_BREP ( 'Thread1', #1623 ) ;
#2807 = CARTESIAN_POINT ( 'NONE',  ( -19.39806930854667755, 4.649999998907525800, -19.39806930854668110 ) ) ;
#2808 = CARTESIAN_POINT ( 'NONE',  ( -10.49999999999999822, 104.5000000000000142, 0.000000000000000000 ) ) ;
#2809 = VECTOR ( 'NONE', #1255, 1000.000000000000114 ) ;
#2810 = LINE ( 'NONE', #3649, #2757 ) ;
#2811 = ORIENTED_EDGE ( 'NONE', *, *, #2261, .T. ) ;
#2812 = DIRECTION ( 'NONE',  ( 0.000000000000000000, 1.000000000000000000, -0.000000000000000000 ) ) ;
#2813 = FACE_BOUND ( 'NONE', #1488, .T. ) ;
#2814 = EDGE_CURVE ( 'NONE', #6040, #7000, #6643, .T. ) ;
#2815 = DIRECTION ( 'NONE',  ( 0.2907756355032780071, 0.000000000000000000, 0.9567912676219745283 ) ) ;
#2816 = CARTESIAN_POINT ( 'NONE',  ( -16.36254897777739004, 99.50000000000001421, 15.39785597259249350 ) ) ;
#2817 = CARTESIAN_POINT ( 'NONE',  ( 3.573144549190039321, 99.99999999999998579, -23.04580706645134214 ) ) ;
#2818 = EDGE_CURVE ( 'NONE', #6584, #7275, #10319, .T. ) ;
#2819 = EDGE_LOOP ( 'NONE', ( #8359, #4591, #5070, #10010 ) ) ;
#2820 = CARTESIAN_POINT ( 'NONE',  ( 4.773458297025112707, 100.0000000000000142, -24.02094923175124208 ) ) ;
#2821 = CARTESIAN_POINT ( 'NONE',  ( -27.43301270000000258, 2.349999998907525534, -3.359575119402369376E-15 ) ) ;
#2822 = ORIENTED_EDGE ( 'NONE', *, *, #10192, .F. ) ;
#2823 = B_SPLINE_CURVE_WITH_KNOTS ( 'NONE', 3,
 ( #9488, #8016, #9681, #3301, #5609, #896, #2312, #5512, #4037, #4765, #4085, #1523, #8062, #4716, #1679 ),
 .UNSPECIFIED., .F., .F.,
 ( 4, 1, 1, 1, 1, 1, 1, 1, 1, 1, 1, 1, 4 ),
 ( 0.000000000000000000, 0.08595325681623211533, 0.1695367914770939399, 0.2510169726856145700, 0.3324720360531058239, 0.4139176782331075444, 0.4946662699496591764, 0.5765962148649595997, 0.6610575120797289594, 0.7465372922784411225, 0.8302848992160567487, 0.9144215288650135998, 1.000000000000000000 ),
 .UNSPECIFIED. ) ;
#2824 = CARTESIAN_POINT ( 'NONE',  ( 2.500000000000000000, -1.987499999999999600, -1.443375672974064994 ) ) ;
#2825 = DIRECTION ( 'NONE',  ( 0.000000000000000000, 0.000000000000000000, 1.000000000000000000 ) ) ;
#2826 = CARTESIAN_POINT ( 'NONE',  ( -3.486133158594716510E-16, -3.712499999999999467, -2.500000000000000000 ) ) ;
#2827 = CARTESIAN_POINT ( 'NONE',  ( 1.128215178125001161, -2.353124999385482585, 1.954126010382870815 ) ) ;
#2828 = CARTESIAN_POINT ( 'NONE',  ( -27.43301270000000258, 2.999999998907525445, -11.36312591709336317 ) ) ;
#2829 = DIRECTION ( 'NONE',  ( 0.000000000000000000, 1.000000000000000000, 0.000000000000000000 ) ) ;
#2830 = VERTEX_POINT ( 'NONE', #5460 ) ;
#2831 = CARTESIAN_POINT ( 'NONE',  ( 3.888553205800344248, 99.99999999999995737, -24.35333287445124739 ) ) ;
#2832 = FACE_OUTER_BOUND ( 'NONE', #1997, .T. ) ;
#2833 = FACE_OUTER_BOUND ( 'NONE', #1989, .T. ) ;
#2834 = CARTESIAN_POINT ( 'NONE',  ( -1.595409442497313560E-16, -2.503124999385482496, -2.605501347177161087 ) ) ;
#2835 = CARTESIAN_POINT ( 'NONE',  ( -0.6698729810778105698, -3.957596189432334377, 2.499999999999997780 ) ) ;
#2836 = ORIENTED_EDGE ( 'NONE', *, *, #6874, .F. ) ;
#2837 =( BOUNDED_CURVE ( )  B_SPLINE_CURVE ( 2, ( #2826, #4547, #524, #6170, #3044, #5340, #5218, #4659, #7627 ),
 .UNSPECIFIED., .F., .T. ) 
 B_SPLINE_CURVE_WITH_KNOTS ( ( 3, 2, 2, 2, 3 ),
 ( 0.6875000000000000000, 0.6944444444444444198, 0.7083333333333333703, 0.7222222222222222099, 0.7291666666666667407 ),
 .UNSPECIFIED. ) 
 CURVE ( )  GEOMETRIC_REPRESENTATION_ITEM ( )  RATIONAL_B_SPLINE_CURVE ( ( 0.9330127018922194093, 0.9330127018922194093, 1.000000000000000000, 0.8660254037844387076, 1.000000000000000000, 0.8660254037844387076, 1.000000000000000000, 0.9330127018922187432, 0.9330127018922192983 ) ) 
 REPRESENTATION_ITEM ( '' )  );
#2838 = CARTESIAN_POINT ( 'NONE',  ( 27.43301270000000258, 3.499999998907525445, -11.36312591709336139 ) ) ;
#2839 = CARTESIAN_POINT ( 'NONE',  ( -1.249999999999998224, -1.668749998770965970, 2.165063509461097713 ) ) ;
#2840 = LINE ( 'NONE', #8436, #7947 ) ;
#2841 = DIRECTION ( 'NONE',  ( -0.000000000000000000, 1.000000000000000000, -0.000000000000000000 ) ) ;
#2842 = ORIENTED_EDGE ( 'NONE', *, *, #1493, .T. ) ;
#2843 = CARTESIAN_POINT ( 'NONE',  ( 6.246869686064662197, 100.0000000000000000, 20.92172973853146090 ) ) ;
#2844 = CARTESIAN_POINT ( 'NONE',  ( -2.256430356250000102, -2.540624999385482141, -1.302750673588580321 ) ) ;
#2845 = ORIENTED_EDGE ( 'NONE', *, *, #4349, .T. ) ;
#2846 = CARTESIAN_POINT ( 'NONE',  ( -22.21584973381871464, 99.99999999999998579, -9.938501092090024969 ) ) ;
#2847 = LINE ( 'NONE', #9221, #9794 ) ;
#2848 = CARTESIAN_POINT ( 'NONE',  ( -27.00000000000001421, 5.049999997815051600, 11.18376618407356560 ) ) ;
#2849 = CARTESIAN_POINT ( 'NONE',  ( 4.988497440555089923, 100.0000000000000284, -24.29977663856455194 ) ) ;
#2850 = EDGE_CURVE ( 'NONE', #7023, #8336, #5348, .T. ) ;
#2851 = ADVANCED_FACE ( 'NONE', ( #10321, #3724 ), #3106, .T. ) ;
#2852 = CARTESIAN_POINT ( 'NONE',  ( 5.302876193624534821E-16, -0.7312499987709658589, 2.886751345948128655 ) ) ;
#2853 = CARTESIAN_POINT ( 'NONE',  ( -2.500000000000000000, -2.681249998770965259, -1.443375672974064106 ) ) ;
#2854 = CARTESIAN_POINT ( 'NONE',  ( 7.486453019397995234, 99.50000000000000000, 23.81666162955709964 ) ) ;
#2855 = ORIENTED_EDGE ( 'NONE', *, *, #2909, .F. ) ;
#2856 = CARTESIAN_POINT ( 'NONE',  ( -1.002171269888535572E-15, -20.00000000000000000, 2.958985580760426615 ) ) ;
#2857 = CARTESIAN_POINT ( 'NONE',  ( 27.43301270000000258, 4.349999998907525089, 0.000000000000000000 ) ) ;
#2858 = CARTESIAN_POINT ( 'NONE',  ( 3.282077632710153292, 99.50000000000000000, -23.74569985055724786 ) ) ;
#2859 = CARTESIAN_POINT ( 'NONE',  ( 9.881472129446523311, 100.0000000000000142, 20.94326683228310060 ) ) ;
#2860 = EDGE_CURVE ( 'NONE', #3761, #7541, #10218, .T. ) ;
#2861 = ADVANCED_FACE ( 'NONE', ( #3775 ), #582, .F. ) ;
#2862 = ORIENTED_EDGE ( 'NONE', *, *, #6832, .F. ) ;
#2863 = CARTESIAN_POINT ( 'NONE',  ( -21.59614764830937972, 100.0000000000000142, -9.292069227195950631 ) ) ;
#2864 = CARTESIAN_POINT ( 'NONE',  ( 5.047889085735837611, 99.50000000000001421, -24.22022158424849536 ) ) ;
#2865 = CARTESIAN_POINT ( 'NONE',  ( 19.09188309203678813, 3.299999999999999822, -19.09188309203678813 ) ) ;
#2866 = DIRECTION ( 'NONE',  ( 0.000000000000000000, 0.000000000000000000, -1.000000000000000000 ) ) ;
#2867 = CARTESIAN_POINT ( 'NONE',  ( -1.250000000000000222, -0.5250000000000000222, -2.165063509461096825 ) ) ;
#2868 = ORIENTED_EDGE ( 'NONE', *, *, #521, .F. ) ;
#2869 = CARTESIAN_POINT ( 'NONE',  ( -16.56928979259283352, 99.50000000000002842, 16.65656195153832897 ) ) ;
#2870 = VECTOR ( 'NONE', #5879, 1000.000000000000000 ) ;
#2871 = CARTESIAN_POINT ( 'NONE',  ( -11.36312591709335962, 2.199999998907525622, -27.43301270000000258 ) ) ;
#2872 = ORIENTED_EDGE ( 'NONE', *, *, #5787, .F. ) ;
#2873 = CARTESIAN_POINT ( 'NONE',  ( -1.250000000000000222, -1.875000000000000000, -2.165063509461096825 ) ) ;
#2874 = CARTESIAN_POINT ( 'NONE',  ( 3.428579745388047328, 99.99999999999995737, -21.16399209792802694 ) ) ;
#2875 = CARTESIAN_POINT ( 'NONE',  ( -1.595409442497313560E-16, -2.165624999385483029, -2.605501347177161087 ) ) ;
#2876 = CARTESIAN_POINT ( 'NONE',  ( 1.679787559701184688E-15, 4.449999998907525622, -27.43301270000000258 ) ) ;
#2877 = VERTEX_POINT ( 'NONE', #2359 ) ;
#2878 = CARTESIAN_POINT ( 'NONE',  ( 19.39806930854668110, 2.049999998907525711, -19.39806930854668110 ) ) ;
#2880 = VERTEX_POINT ( 'NONE', #2311 ) ;
#2879 = ORIENTED_EDGE ( 'NONE', *, *, #1907, .T. ) ;
#2881 = CIRCLE ( 'NONE', #8073, 2.500000000000000000 ) ;
#2882 = CARTESIAN_POINT ( 'NONE',  ( 9.526349065647009340, 100.0000000000000000, 19.81320455978211470 ) ) ;
#2883 = CARTESIAN_POINT ( 'NONE',  ( -1.249999999999998224, -3.018749998770965615, 2.165063509461097713 ) ) ;
#2884 = CARTESIAN_POINT ( 'NONE',  ( 5.725936192474917696, 100.0000000000000000, 21.08018326417248645 ) ) ;
#2885 = CARTESIAN_POINT ( 'NONE',  ( 3.810791133452845703, 100.0000000000000568, -24.33305202239136733 ) ) ;
#2886 = CARTESIAN_POINT ( 'NONE',  ( -1.128215178124998497, -2.315624999385482941, 1.954126010382872147 ) ) ;
#2887 = CARTESIAN_POINT ( 'NONE',  ( 3.195700652717397894, 99.99999999999997158, -22.66286045753255962 ) ) ;
#2888 = ORIENTED_EDGE ( 'NONE', *, *, #966, .F. ) ;
#2889 = LINE ( 'NONE', #2946, #7395 ) ;
#2890 = CARTESIAN_POINT ( 'NONE',  ( -11.36312591709337383, 1.599999998907525534, 27.43301269999999548 ) ) ;
#2891 = AXIS2_PLACEMENT_3D ( 'NONE', #3504, #8322, #6690 ) ;
#2892 = CARTESIAN_POINT ( 'NONE',  ( 27.43301270000000258, 0.2999999989075251561, 0.000000000000000000 ) ) ;
#2893 = EDGE_CURVE ( 'NONE', #669, #7666, #7065, .T. ) ;
#2894 = CARTESIAN_POINT ( 'NONE',  ( -19.09188309203678457, 0.3000000000000000444, -19.09188309203678813 ) ) ;
#2895 = CARTESIAN_POINT ( 'NONE',  ( 9.245739950628269810, 100.0000000000000568, 20.03726560014620617 ) ) ;
#2896 = VERTEX_POINT ( 'NONE', #1362 ) ;
#2897 = ORIENTED_EDGE ( 'NONE', *, *, #6076, .T. ) ;
#2898 = CARTESIAN_POINT ( 'NONE',  ( 4.739008722453744049, 100.0000000000000142, -24.06821587619827696 ) ) ;
#2899 = MECHANICAL_DESIGN_GEOMETRIC_PRESENTATION_REPRESENTATION (  '', ( #7077 ), #4740 ) ;
#2900 = CARTESIAN_POINT ( 'NONE',  ( 4.786228327491941173E-16, -1.940624999385482718, 2.605501347177161087 ) ) ;
#2901 = EDGE_LOOP ( 'NONE', ( #5884, #1557, #3818, #6823, #2249, #732, #8229, #3585 ) ) ;
#2902 = CARTESIAN_POINT ( 'NONE',  ( -22.06741020400400188, 99.50000000000004263, -9.788922322134999021 ) ) ;
#2903 = CARTESIAN_POINT ( 'NONE',  ( -15.45548338988150938, 99.99999999999997158, 16.93306818456458984 ) ) ;
#2904 = CARTESIAN_POINT ( 'NONE',  ( -20.96643530928959365, 99.50000000000000000, -10.05541671241504886 ) ) ;
#2905 = CARTESIAN_POINT ( 'NONE',  ( 2.256430356250000546, -0.9656249993854827407, 1.302750673588579877 ) ) ;
#2906 = CARTESIAN_POINT ( 'NONE',  ( 5.098880966732203035, 100.0000000000000284, -24.13374913903897223 ) ) ;
#2907 = ORIENTED_EDGE ( 'NONE', *, *, #9087, .F. ) ;
#2908 = CARTESIAN_POINT ( 'NONE',  ( 4.504418077186241653, 99.50000000000004263, -21.31258943653750393 ) ) ;
#2909 = EDGE_CURVE ( 'NONE', #7789, #969, #1804, .T. ) ;
#2910 = CARTESIAN_POINT ( 'NONE',  ( 0.000000000000000000, 0.000000000000000000, 0.000000000000000000 ) ) ;
#2911 = CARTESIAN_POINT ( 'NONE',  ( 9.526713201929464248, 100.0000000000000000, 20.38668308130821671 ) ) ;
#2912 = ORIENTED_EDGE ( 'NONE', *, *, #8427, .F. ) ;
#2913 = PLANE ( 'NONE',  #8914 ) ;
#2914 = CARTESIAN_POINT ( 'NONE',  ( 19.39806930854668110, 4.449999998907525622, -19.39806930854668110 ) ) ;
#2915 = CARTESIAN_POINT ( 'NONE',  ( -2.256430356249999214, -1.453124999385482896, 1.302750673588581876 ) ) ;
#2916 = CARTESIAN_POINT ( 'NONE',  ( 9.897596448871711416, 99.49999999999998579, 20.85734708541456328 ) ) ;
#2917 = CIRCLE ( 'NONE', #5075, 25.15000000000000213 ) ;
#2918 = B_SPLINE_SURFACE_WITH_KNOTS ( 'NONE', 3, 1, ( 
 ( #3415, #2590 ),
 ( #9853, #4163 ),
 ( #5781, #6610 ),
 ( #7439, #1795 ),
 ( #9905, #8188 ),
 ( #1016, #8285 ),
 ( #5926, #4208 ),
 ( #4258, #1118 ),
 ( #1746, #2689 ),
 ( #4308, #2639 ),
 ( #9023, #5831 ),
 ( #1840, #5878 ),
 ( #7347, #7392 ),
 ( #7493, #5035 ),
 ( #9077, #4942 ),
 ( #1066, #183 ),
 ( #6563, #8235 ),
 ( #3369, #9754 ),
 ( #332, #7545 ) ),
 .UNSPECIFIED., .F., .F., .F.,
 ( 4, 1, 1, 1, 1, 1, 1, 1, 1, 1, 1, 1, 1, 1, 1, 1, 4 ),
 ( 2, 2 ),
 ( 0.000000000000000000, 0.05935611633690887623, 0.1167563879513689451, 0.1743885027374874330, 0.2308223543163396840, 0.2888100779544915953, 0.3475404098195560842, 0.4086537266250744316, 0.4723446836969566465, 0.5362968130936018873, 0.6000923674009760456, 0.6637702377379335328, 0.7274568328636339398, 0.7924602533659969028, 0.8590386936388050287, 0.9283644560612371865, 1.000000000000000000 ),
 ( 0.000000000000000000, 1.000000000000000000 ),
 .UNSPECIFIED. ) ;
#2919 = CARTESIAN_POINT ( 'NONE',  ( -16.07368679829020763, 99.50000000000000000, 17.11560437002838952 ) ) ;
#2920 = CARTESIAN_POINT ( 'NONE',  ( 0.000000000000000000, 85.00000000000000000, 0.000000000000000000 ) ) ;
#2921 = CARTESIAN_POINT ( 'NONE',  ( 0.000000000000000000, 0.000000000000000000, -2.500000000000000000 ) ) ;
#2922 = FACE_OUTER_BOUND ( 'NONE', #4194, .T. ) ;
#2923 = EDGE_LOOP ( 'NONE', ( #7895, #6101 ) ) ;
#2924 = CARTESIAN_POINT ( 'NONE',  ( -15.76955986605724647, 99.99999999999998579, 15.18352214517458698 ) ) ;
#2925 = CARTESIAN_POINT ( 'NONE',  ( 27.43301269999999548, 2.699999998907525178, 11.36312591709337916 ) ) ;
#2926 = VERTEX_POINT ( 'NONE', #2465 ) ;
#2927 = EDGE_CURVE ( 'NONE', #9400, #1992, #951, .T. ) ;
#2928 = CARTESIAN_POINT ( 'NONE',  ( 2.500000000000000000, -1.537499999999999645, -1.443375672974064994 ) ) ;
#2929 = AXIS2_PLACEMENT_3D ( 'NONE', #7685, #2990, #10209 ) ;
#2930 = DIRECTION ( 'NONE',  ( 1.000000000000000000, 0.000000000000000000, 0.000000000000000000 ) ) ;
#2931 = CARTESIAN_POINT ( 'NONE',  ( 9.502908418173033667, 99.50000000000000000, 20.32929868008965002 ) ) ;
#2932 = CARTESIAN_POINT ( 'NONE',  ( -7.500000000000000888, 104.5000000000000142, 3.000000000000000000 ) ) ;
#2933 = CARTESIAN_POINT ( 'NONE',  ( 4.786228327491941173E-16, -2.840624999385482852, 2.605501347177161087 ) ) ;
#2934 = CARTESIAN_POINT ( 'NONE',  ( 11.18376618407357093, 0.7499999978150503344, -27.00000000000000355 ) ) ;
#2935 = CARTESIAN_POINT ( 'NONE',  ( 27.43301270000000258, 2.749999998907525445, 0.000000000000000000 ) ) ;
#2936 = ORIENTED_EDGE ( 'NONE', *, *, #2624, .T. ) ;
#2937 = CARTESIAN_POINT ( 'NONE',  ( 9.806436918512124734, 99.99999999999998579, 20.18080982695387604 ) ) ;
#2938 = CARTESIAN_POINT ( 'NONE',  ( 3.970307086022987431, 100.0000000000000142, -24.36314111580913178 ) ) ;
#2939 = CARTESIAN_POINT ( 'NONE',  ( -16.36470918167357169, 99.50000000000000000, 16.79054296464299867 ) ) ;
#2940 = AXIS2_PLACEMENT_3D ( 'NONE', #2776, #4147, #9782 ) ;
#2941 = CARTESIAN_POINT ( 'NONE',  ( -15.76955986605724647, 99.99999999999998579, 15.18352214517458698 ) ) ;
#2942 = EDGE_LOOP ( 'NONE', ( #2208, #5704 ) ) ;
#2943 = CARTESIAN_POINT ( 'NONE',  ( -1.595409442497313560E-16, -2.053124999385482763, -2.605501347177161087 ) ) ;
#2944 = CARTESIAN_POINT ( 'NONE',  ( 3.105863891863242632, 100.0000000000000142, -22.59672720503480292 ) ) ;
#2945 = ORIENTED_EDGE ( 'NONE', *, *, #3693, .F. ) ;
#2946 = CARTESIAN_POINT ( 'NONE',  ( 8.429066232339796017, 99.50000000000000000, 19.67794530653910101 ) ) ;
#2947 = VECTOR ( 'NONE', #5750, 1000.000000000000000 ) ;
#2948 = CARTESIAN_POINT ( 'NONE',  ( 11.36312591709336139, 3.599999998907525089, -27.43301270000000258 ) ) ;
#2949 =( LENGTH_UNIT ( ) NAMED_UNIT ( * ) SI_UNIT ( .MILLI., .METRE. ) );
#2950 = ORIENTED_EDGE ( 'NONE', *, *, #9357, .F. ) ;
#2951 = CARTESIAN_POINT ( 'NONE',  ( 2.500000000000000000, -2.868749998770965703, -3.061616997868383141E-16 ) ) ;
#2952 = CARTESIAN_POINT ( 'NONE',  ( -11.18376618407358336, 2.149999999999999911, 26.99999999999999645 ) ) ;
#2953 = CARTESIAN_POINT ( 'NONE',  ( -9.703070624755296135E-15, -3.881249998770965881, 2.500000000000000444 ) ) ;
#2954 = VERTEX_POINT ( 'NONE', #2565 ) ;
#2955 = CARTESIAN_POINT ( 'NONE',  ( -15.22739782325755442, 99.49999999999998579, 15.50750051783781025 ) ) ;
#2956 = CARTESIAN_POINT ( 'NONE',  ( -15.42956291708403782, 99.49999999999998579, 16.53061251458192515 ) ) ;
#2957 = EDGE_CURVE ( 'NONE', #4542, #4452, #6719, .T. ) ;
#2958 = CARTESIAN_POINT ( 'NONE',  ( -1.595409442497313560E-16, -1.265624999385482896, -2.605501347177161087 ) ) ;
#2959 = ORIENTED_EDGE ( 'NONE', *, *, #2158, .F. ) ;
#2960 = VERTEX_POINT ( 'NONE', #5756 ) ;
#2961 = EDGE_CURVE ( 'NONE', #8960, #8911, #3691, .T. ) ;
#2962 = CARTESIAN_POINT ( 'NONE',  ( 4.259295290443009918, 99.50000000000002842, -24.34414156132068996 ) ) ;
#2963 = CARTESIAN_POINT ( 'NONE',  ( 11.36312591709336139, 0.3999999989075253559, -27.43301270000000258 ) ) ;
#2964 = DIRECTION ( 'NONE',  ( -0.000000000000000000, 1.000000000000000000, -0.000000000000000000 ) ) ;
#2965 = VECTOR ( 'NONE', #6660, 1000.000000000000000 ) ;
#2966 = CARTESIAN_POINT ( 'NONE',  ( 2.256430356249999658, -0.8906249993854827851, -1.302750673588581432 ) ) ;
#2967 = CARTESIAN_POINT ( 'NONE',  ( -19.09188309203678813, 3.700000000000000178, 19.09188309203678457 ) ) ;
#2968 = CARTESIAN_POINT ( 'NONE',  ( -1.249999999999998224, -1.724999999999999645, 2.165063509461097713 ) ) ;
#2969 = CIRCLE ( 'NONE', #6312, 25.00000000000000000 ) ;
#2970 = CARTESIAN_POINT ( 'NONE',  ( 4.034460619503033030, 99.49999999999995737, -21.08676866017170681 ) ) ;
#2971 = FACE_OUTER_BOUND ( 'NONE', #1110, .T. ) ;
#2972 = DIRECTION ( 'NONE',  ( -0.9572638942369904314, 0.000000000000000000, 0.2892158999609669712 ) ) ;
#2973 = ORIENTED_EDGE ( 'NONE', *, *, #4900, .T. ) ;
#2974 = CARTESIAN_POINT ( 'NONE',  ( -4.959819536546781389E-15, 1.199999997815050401, 27.00000000000000355 ) ) ;
#2975 = DIRECTION ( 'NONE',  ( 0.000000000000000000, -1.000000000000000000, 0.000000000000000000 ) ) ;
#2976 = CARTESIAN_POINT ( 'NONE',  ( 1.128215178124999607, -1.190624999385482941, -1.954126010382871259 ) ) ;
#2977 = CARTESIAN_POINT ( 'NONE',  ( 9.692323321704657602, 100.0000000000000000, 21.58969587442354410 ) ) ;
#2978 = VERTEX_POINT ( 'NONE', #8014 ) ;
#2979 = CARTESIAN_POINT ( 'NONE',  ( 1.653273178848927064E-15, 5.599999997815050534, -27.00000000000000355 ) ) ;
#2980 = CARTESIAN_POINT ( 'NONE',  ( 8.857094148306096315, 99.50000000000001421, 19.57755665027156766 ) ) ;
#2981 = CARTESIAN_POINT ( 'NONE',  ( -7.500000000000000000, 104.5000000000000142, -0.9999999999999997780 ) ) ;
#2982 = CARTESIAN_POINT ( 'NONE',  ( -16.41302370085497131, 99.49999999999998579, 15.45185748370271206 ) ) ;
#2983 = VERTEX_POINT ( 'NONE', #6489 ) ;
#2984 = CARTESIAN_POINT ( 'NONE',  ( -16.36470918167357169, 100.0000000000000000, 16.79054296464299867 ) ) ;
#2985 = CARTESIAN_POINT ( 'NONE',  ( -19.39806930854668465, 0.8499999989075252005, 19.39806930854667755 ) ) ;
#2986 = VERTEX_POINT ( 'NONE', #2610 ) ;
#2987 = AXIS2_PLACEMENT_3D ( 'NONE', #2478, #9690, #8908 ) ;
#2988 = CARTESIAN_POINT ( 'NONE',  ( 5.302876193624534821E-16, -3.037499999999999645, 2.886751345948128655 ) ) ;
#2989 =( NAMED_UNIT ( * ) PLANE_ANGLE_UNIT ( ) SI_UNIT ( $, .RADIAN. ) );
#2990 = DIRECTION ( 'NONE',  ( -0.000000000000000000, -1.000000000000000000, -0.000000000000000000 ) ) ;
#2991 = CARTESIAN_POINT ( 'NONE',  ( 2.256430356249999658, -2.690624999385482941, -1.302750673588581432 ) ) ;
#2992 = CARTESIAN_POINT ( 'NONE',  ( -27.43301270000000258, 4.599999998907525978, -11.36312591709336317 ) ) ;
#2993 = CARTESIAN_POINT ( 'NONE',  ( 27.43301269999999548, 3.499999998907525445, 11.36312591709337738 ) ) ;
#2995 = ORIENTED_EDGE ( 'NONE', *, *, #5638, .T. ) ;
#2994 = ORIENTED_EDGE ( 'NONE', *, *, #4290, .T. ) ;
#2996 = PRODUCT_DEFINITION_CONTEXT ( 'detailed design', #451, 'design' ) ;
#2997 = EDGE_CURVE ( 'NONE', #3336, #1808, #4959, .T. ) ;
#2998 = CARTESIAN_POINT ( 'NONE',  ( -20.42657152723830905, 99.50000000000000000, -10.54129411626120216 ) ) ;
#2999 = VECTOR ( 'NONE', #146, 1000.000000000000000 ) ;
#3000 = CARTESIAN_POINT ( 'NONE',  ( 21.82251602564102910, 100.0000000000000000, -0.5181290064102563875 ) ) ;
#3001 = CARTESIAN_POINT ( 'NONE',  ( 3.551917533706515417, 99.50000000000001421, -21.11785906961830150 ) ) ;
#3002 = CARTESIAN_POINT ( 'NONE',  ( 3.535161742238301041, 100.0000000000000142, -24.18247714022527006 ) ) ;
#3003 = ORIENTED_EDGE ( 'NONE', *, *, #5646, .T. ) ;
#3004 = CARTESIAN_POINT ( 'NONE',  ( 2.256430356250000546, -1.303124999385482985, 1.302750673588579877 ) ) ;
#3005 = CARTESIAN_POINT ( 'NONE',  ( 3.948639947730041566, 99.99999999999998579, -21.07692942975820927 ) ) ;
#3006 = ORIENTED_EDGE ( 'NONE', *, *, #1918, .T. ) ;
#3007 = CARTESIAN_POINT ( 'NONE',  ( 1.128215178124999607, -0.2906249993854829738, -1.954126010382871259 ) ) ;
#3008 = CARTESIAN_POINT ( 'NONE',  ( -5.039362679103552881E-15, 1.649999998907525134, 27.43301270000000258 ) ) ;
#3009 = SURFACE_SIDE_STYLE ('',( #5181 ) ) ;
#3010 = CARTESIAN_POINT ( 'NONE',  ( -4.959819536546781389E-15, 3.000000000000000000, 27.00000000000000355 ) ) ;
#3011 = CARTESIAN_POINT ( 'NONE',  ( 27.00000000000000355, 0.05000000000000000278, -11.18376618407356737 ) ) ;
#3012 = CARTESIAN_POINT ( 'NONE',  ( 2.852289972453743161, 99.50000000000000000, -22.14293542748032451 ) ) ;
#3013 = ORIENTED_EDGE ( 'NONE', *, *, #2379, .F. ) ;
#3014 = CARTESIAN_POINT ( 'NONE',  ( -16.52319226728147328, 99.49999999999998579, 15.63609008536095324 ) ) ;
#3015 = CARTESIAN_POINT ( 'NONE',  ( -15.69015368034045643, 100.0000000000000142, 16.64011368054243434 ) ) ;
#3016 = VERTEX_POINT ( 'NONE', #53 ) ;
#3017 = CARTESIAN_POINT ( 'NONE',  ( -2.256430356250000102, -4.303124999385482319, 0.000000000000000000 ) ) ;
#3018 = EDGE_LOOP ( 'NONE', ( #5288, #5280 ) ) ;
#3019 = ORIENTED_EDGE ( 'NONE', *, *, #1880, .F. ) ;
#3020 = CARTESIAN_POINT ( 'NONE',  ( 9.877377282685029372E-16, -0.7874999999999998668, 2.500000000000000000 ) ) ;
#3021 = LINE ( 'NONE', #3071, #3525 ) ;
#3022 = PRODUCT ( 'grease nipple', 'grease nipple', '', ( #572 ) ) ;
#3023 = PRODUCT_RELATED_PRODUCT_CATEGORY ( 'part', '', ( #3022 ) ) ;
#3024 = CARTESIAN_POINT ( 'NONE',  ( -2.256430356250000102, -1.603124999385482807, 0.000000000000000000 ) ) ;
#3025 = CARTESIAN_POINT ( 'NONE',  ( 5.047889085735837611, 100.0000000000000426, -24.22022158424849536 ) ) ;
#3026 = DIRECTION ( 'NONE',  ( 0.000000000000000000, -0.000000000000000000, -1.000000000000000000 ) ) ;
#3027 = EDGE_CURVE ( 'NONE', #9293, #647, #203, .T. ) ;
#3028 = CARTESIAN_POINT ( 'NONE',  ( 5.302876193624534821E-16, -2.081249998770965171, 2.886751345948128655 ) ) ;
#3029 = ADVANCED_FACE ( 'NONE', ( #4871 ), #8060, .T. ) ;
#3030 = DIRECTION ( 'NONE',  ( -1.000000000000000000, 0.000000000000000000, 0.000000000000000000 ) ) ;
#3031 = CARTESIAN_POINT ( 'NONE',  ( 1.653273178848927064E-15, 2.600000000000000533, -27.00000000000000355 ) ) ;
#3032 = ORIENTED_EDGE ( 'NONE', *, *, #624, .T. ) ;
#3033 = CARTESIAN_POINT ( 'NONE',  ( 9.676361905416719367, 100.0000000000000000, 21.63547735782115211 ) ) ;
#3034 = CARTESIAN_POINT ( 'NONE',  ( -2.256430356250000102, -1.940624999385482941, 0.000000000000000000 ) ) ;
#3035 = EDGE_CURVE ( 'NONE', #6279, #2600, #10191, .T. ) ;
#3036 = DIRECTION ( 'NONE',  ( -0.000000000000000000, 1.000000000000000000, -0.000000000000000000 ) ) ;
#3037 = CARTESIAN_POINT ( 'NONE',  ( -1.915120254295647362, -5.000523192925935945, -1.606958123781256464 ) ) ;
#3038 = CARTESIAN_POINT ( 'NONE',  ( -16.52319226728147328, 99.49999999999998579, 15.63609008536095324 ) ) ;
#3039 = ORIENTED_EDGE ( 'NONE', *, *, #80, .F. ) ;
#3040 = CARTESIAN_POINT ( 'NONE',  ( -16.33590634957226229, 99.50000000000000000, 16.80570853669505382 ) ) ;
#3041 = CARTESIAN_POINT ( 'NONE',  ( -27.43301270000000258, 0.7499999989075251117, -3.359575119402369376E-15 ) ) ;
#3042 = VERTEX_POINT ( 'NONE', #8992 ) ;
#3043 = CARTESIAN_POINT ( 'NONE',  ( 1.249999999999999334, -4.200000000000000178, -2.165063509461096825 ) ) ;
#3044 = CARTESIAN_POINT ( 'NONE',  ( 2.500000000000000000, -3.824999999999999734, -3.061616997868383141E-16 ) ) ;
#3045 = CARTESIAN_POINT ( 'NONE',  ( -1.128215178125000273, -0.7781249993854828517, -1.954126010382871259 ) ) ;
#3046 = CARTESIAN_POINT ( 'NONE',  ( 27.43301270000000258, 5.099999998907525978, -11.36312591709336139 ) ) ;
#3047 = CARTESIAN_POINT ( 'NONE',  ( -27.43301270000000258, 2.349999998907525534, -3.359575119402369376E-15 ) ) ;
#3048 = CARTESIAN_POINT ( 'NONE',  ( 9.666415885916139317, 100.0000000000000142, 19.95264712196244261 ) ) ;
#3049 = CARTESIAN_POINT ( 'NONE',  ( -2.499999999999999112, -3.056249998770965703, 1.443375672974065882 ) ) ;
#3050 = DIRECTION ( 'NONE',  ( 0.000000000000000000, -0.000000000000000000, 1.000000000000000000 ) ) ;
#3051 = DIRECTION ( 'NONE',  ( 0.000000000000000000, -1.000000000000000000, 0.000000000000000000 ) ) ;
#3052 = CARTESIAN_POINT ( 'NONE',  ( -1.128215178124998497, -0.9656249993854828517, 1.954126010382872147 ) ) ;
#3053 = LINE ( 'NONE', #9584, #4947 ) ;
#3054 = ORIENTED_EDGE ( 'NONE', *, *, #6738, .T. ) ;
#3055 = ADVANCED_FACE ( 'NONE', ( #9193 ), #8257, .F. ) ;
#3056 = CARTESIAN_POINT ( 'NONE',  ( -1.595409442497313560E-16, -1.603124999385482807, -2.605501347177161087 ) ) ;
#3057 = CARTESIAN_POINT ( 'NONE',  ( -27.43301270000000258, 1.399999998907525134, -11.36312591709336317 ) ) ;
#3058 = DIRECTION ( 'NONE',  ( 0.000000000000000000, 1.000000000000000000, 0.000000000000000000 ) ) ;
#3059 = AXIS2_PLACEMENT_3D ( 'NONE', #5619, #8121, #952 ) ;
#3060 = CARTESIAN_POINT ( 'NONE',  ( -27.00000000000000355, 0.3499999999999999778, -11.18376618407357093 ) ) ;
#3061 = CARTESIAN_POINT ( 'NONE',  ( 9.182805720491336032, 100.0000000000000284, 20.00174565872165289 ) ) ;
#3062 = ORIENTED_EDGE ( 'NONE', *, *, #3625, .F. ) ;
#3063 =( BOUNDED_CURVE ( )  B_SPLINE_CURVE ( 2, ( #941, #4134, #7317, #155, #9191, #9980, #2865, #8356, #2129 ),
 .UNSPECIFIED., .F., .F. ) 
 B_SPLINE_CURVE_WITH_KNOTS ( ( 3, 2, 2, 2, 3 ),
 ( 0.5357142857142856984, 0.5535714285714286031, 0.5714285714285713969, 0.5892857142857143016, 0.6071428571428570953 ),
 .UNSPECIFIED. ) 
 CURVE ( )  GEOMETRIC_REPRESENTATION_ITEM ( )  RATIONAL_B_SPLINE_CURVE ( ( 1.000000000000000000, 0.9238795325112867385, 1.000000000000000000, 0.9238795325112867385, 1.000000000000000000, 0.9238795325112867385, 1.000000000000000000, 0.9238795325112867385, 1.000000000000000000 ) ) 
 REPRESENTATION_ITEM ( '' )  );
#3064 = LINE ( 'NONE', #1434, #8339 ) ;
#3065 = CARTESIAN_POINT ( 'NONE',  ( -15.76250887235353737, 99.99999999999998579, 16.65066592061022277 ) ) ;
#3066 = CARTESIAN_POINT ( 'NONE',  ( -1.128215178124998497, -4.228124999385482141, 1.954126010382872147 ) ) ;
#3067 = ORIENTED_EDGE ( 'NONE', *, *, #2486, .F. ) ;
#3068 = ORIENTED_EDGE ( 'NONE', *, *, #8817, .T. ) ;
#3069 = CIRCLE ( 'NONE', #10254, 25.15000000000000213 ) ;
#3070 = CARTESIAN_POINT ( 'NONE',  ( 19.39806930854667399, 4.149999998907525800, 19.39806930854668465 ) ) ;
#3071 = CARTESIAN_POINT ( 'NONE',  ( -16.07368679829020763, 99.50000000000000000, 17.11560437002838952 ) ) ;
#3072 = EDGE_CURVE ( 'NONE', #7399, #9350, #8305, .T. ) ;
#3073 = CARTESIAN_POINT ( 'NONE',  ( -2.256430356249998770, -1.115624999385482763, 1.302750673588581876 ) ) ;
#3074 = DIRECTION ( 'NONE',  ( -0.000000000000000000, -0.000000000000000000, -1.000000000000000000 ) ) ;
#3075 = CARTESIAN_POINT ( 'NONE',  ( 0.000000000000000000, 71.18660744634364335, 0.000000000000000000 ) ) ;
#3076 = AXIS2_PLACEMENT_3D ( 'NONE', #9135, #3483, #3698 ) ;
#3077 = CARTESIAN_POINT ( 'NONE',  ( -2.500000000000000000, -1.293749998770965970, 0.000000000000000000 ) ) ;
#3078 = ORIENTED_EDGE ( 'NONE', *, *, #4198, .T. ) ;
#3079 = CARTESIAN_POINT ( 'NONE',  ( 4.633286773149219329, 100.0000000000000284, -21.44575434969419447 ) ) ;
#3080 = CARTESIAN_POINT ( 'NONE',  ( -15.07178375341841381, 99.50000000000000000, 16.66969090848992607 ) ) ;
#3081 = ORIENTED_EDGE ( 'NONE', *, *, #9187, .F. ) ;
#3082 = PRESENTATION_LAYER_ASSIGNMENT (  '', '', ( #6248 ) ) ;
#3083 = CARTESIAN_POINT ( 'NONE',  ( 8.961048541867139505, 99.50000000000001421, 19.57961630251783092 ) ) ;
#3084 = CARTESIAN_POINT ( 'NONE',  ( 4.786228327491941173E-16, -1.828124999385482896, 2.605501347177161087 ) ) ;
#3085 = ORIENTED_EDGE ( 'NONE', *, *, #4556, .T. ) ;
#3086 = ORIENTED_EDGE ( 'NONE', *, *, #3800, .F. ) ;
#3087 = CARTESIAN_POINT ( 'NONE',  ( -21.96365545856212265, 100.0000000000000142, -9.726658277667754149 ) ) ;
#3088 = CARTESIAN_POINT ( 'NONE',  ( 9.666415885916139317, 99.50000000000001421, 19.95264712196244261 ) ) ;
#3089 = CARTESIAN_POINT ( 'NONE',  ( 0.000000000000000000, -15.00000000000000000, -3.464101615137755275 ) ) ;
#3090 = CARTESIAN_POINT ( 'NONE',  ( -22.31230063665282515, 99.49999999999997158, -10.62159318200525249 ) ) ;
#3091 = EDGE_CURVE ( 'NONE', #1371, #7818, #8081, .T. ) ;
#3092 = EDGE_LOOP ( 'NONE', ( #3195, #6140, #2450, #3081, #1778, #8606 ) ) ;
#3093 = CARTESIAN_POINT ( 'NONE',  ( -14.78677372028383097, 99.49999999999998579, 15.63810349997947569 ) ) ;
#3094 = CARTESIAN_POINT ( 'NONE',  ( -11.36312591709337561, 4.099999998907525089, 27.43301269999999548 ) ) ;
#3095 = ORIENTED_EDGE ( 'NONE', *, *, #1253, .F. ) ;
#3096 = ADVANCED_FACE ( 'NONE', ( #5954 ), #9146, .T. ) ;
#3097 = CARTESIAN_POINT ( 'NONE',  ( -2.500000000000000000, -3.149999999999999467, 0.000000000000000000 ) ) ;
#3098 = CARTESIAN_POINT ( 'NONE',  ( 3.252389375388976323, 100.0000000000000426, -22.22144413113850447 ) ) ;
#3099 = CARTESIAN_POINT ( 'NONE',  ( -2.256430356250000102, -4.790624999385483029, -1.302750673588580321 ) ) ;
#3100 = CARTESIAN_POINT ( 'NONE',  ( 4.750280232731688201, 99.50000000000002842, -24.05275076595185624 ) ) ;
#3101 = CARTESIAN_POINT ( 'NONE',  ( -27.43301270000000969, 1.599999998907525534, 11.36312591709335429 ) ) ;
#3102 = MANIFOLD_SOLID_BREP ( 'Sweep1', #1780 ) ;
#3103 = PRODUCT_DEFINITION_CONTEXT ( 'detailed design', #10152, 'design' ) ;
#3104 = FACE_OUTER_BOUND ( 'NONE', #6266, .T. ) ;
#3105 = LINE ( 'NONE', #7960, #3318 ) ;
#3106 = PLANE ( 'NONE',  #379 ) ;
#3107 = B_SPLINE_SURFACE_WITH_KNOTS ( 'NONE', 3, 1, ( 
 ( #5974, #9166 ),
 ( #10004, #1986 ),
 ( #4406, #9012 ),
 ( #7589, #427 ),
 ( #3406, #5234 ),
 ( #5026, #4248 ),
 ( #1320, #6077 ),
 ( #7865, #1266 ),
 ( #6186, #9326 ),
 ( #2319, #6297 ),
 ( #3888, #3677 ),
 ( #3839, #6860 ),
 ( #4455, #540 ),
 ( #4509, #7024 ),
 ( #9268, #7076 ) ),
 .UNSPECIFIED., .F., .F., .F.,
 ( 4, 1, 1, 1, 1, 1, 1, 1, 1, 1, 1, 1, 4 ),
 ( 2, 2 ),
 ( 0.000000000000000000, 0.08635447908391848115, 0.1695936995346988552, 0.2509241109261274860, 0.3325843554298174576, 0.4138183564518133073, 0.4948404748415979881, 0.5772065644957810049, 0.6619893985813737336, 0.7474108716807353892, 0.8313115314839791825, 0.9147691218156368542, 1.000000000000000000 ),
 ( 0.000000000000000000, 1.000000000000000000 ),
 .UNSPECIFIED. ) ;
#3108 = CARTESIAN_POINT ( 'NONE',  ( 3.000000000000000000, -15.00000000000000000, -1.732050807568876749 ) ) ;
#3109 = CARTESIAN_POINT ( 'NONE',  ( 2.256430356250000102, -4.865624999385482319, -2.763330213280484622E-16 ) ) ;
#3110 = CARTESIAN_POINT ( 'NONE',  ( -21.89277277937676303, 99.49999999999998579, -9.329958722595300458 ) ) ;
#3111 = VERTEX_POINT ( 'NONE', #3600 ) ;
#3112 = ORIENTED_EDGE ( 'NONE', *, *, #1493, .F. ) ;
#3113 = CARTESIAN_POINT ( 'NONE',  ( 2.256430356249999658, -2.128124999385482941, -1.302750673588581432 ) ) ;
#3114 = CARTESIAN_POINT ( 'NONE',  ( -11.36312591709335962, 2.199999998907525622, -27.43301270000000258 ) ) ;
#3115 = CARTESIAN_POINT ( 'NONE',  ( 0.000000000000000000, 5.000000000000004441, -27.00000000000000355 ) ) ;
#3116 = CARTESIAN_POINT ( 'NONE',  ( -19.09188309203678457, 1.100000000000000089, -19.09188309203678813 ) ) ;
#3117 = CARTESIAN_POINT ( 'NONE',  ( 0.000000000000000000, -5.000000000000000000, 0.000000000000000000 ) ) ;
#3118 = ORIENTED_EDGE ( 'NONE', *, *, #1609, .F. ) ;
#3119 = VECTOR ( 'NONE', #6845, 1000.000000000000000 ) ;
#3120 = CARTESIAN_POINT ( 'NONE',  ( -16.54512803120131181, 99.50000000000000000, 16.13427955854364626 ) ) ;
#3121 = CARTESIAN_POINT ( 'NONE',  ( 8.399337394135656609, 99.49999999999998579, 20.06291166101774692 ) ) ;
#3122 = CARTESIAN_POINT ( 'NONE',  ( -1.595409442497313560E-16, -3.065624999385482496, -2.605501347177161087 ) ) ;
#3123 = VERTEX_POINT ( 'NONE', #3655 ) ;
#3124 = CARTESIAN_POINT ( 'NONE',  ( -27.43301270000000258, 3.049999998907525267, -3.359575119402369376E-15 ) ) ;
#3125 = CARTESIAN_POINT ( 'NONE',  ( 3.061616997868383141E-16, 0.000000000000000000, 2.500000000000000000 ) ) ;
#3126 = CARTESIAN_POINT ( 'NONE',  ( -2.256430356250000102, -1.153124999385482852, 0.000000000000000000 ) ) ;
#3127 = CARTESIAN_POINT ( 'NONE',  ( -11.18376618407358336, 1.949999997815050401, 26.99999999999999645 ) ) ;
#3128 = ORIENTED_EDGE ( 'NONE', *, *, #103, .F. ) ;
#3129 = DIRECTION ( 'NONE',  ( 0.000000000000000000, 0.000000000000000000, 1.000000000000000000 ) ) ;
#3130 = ADVANCED_FACE ( 'NONE', ( #3543 ), #6629, .T. ) ;
#3131 = CARTESIAN_POINT ( 'NONE',  ( 2.500000000000000000, -1.031249998770965792, -1.443375672974064994 ) ) ;
#3132 = VECTOR ( 'NONE', #4793, 1000.000000000000000 ) ;
#3133 = CARTESIAN_POINT ( 'NONE',  ( 4.691018317478480526, 99.99999999999995737, -21.52316599815148024 ) ) ;
#3134 = CARTESIAN_POINT ( 'NONE',  ( -15.89341924297059094, 100.0000000000000142, 17.07725933521297890 ) ) ;
#3135 = CARTESIAN_POINT ( 'NONE',  ( 1.250000000000001110, -4.349999999999999645, 2.165063509461096380 ) ) ;
#3136 = CARTESIAN_POINT ( 'NONE',  ( -1.595409442497313560E-16, -2.503124999385482496, -2.605501347177161087 ) ) ;
#3137 = ORIENTED_EDGE ( 'NONE', *, *, #3357, .T. ) ;
#3138 = DIRECTION ( 'NONE',  ( -1.000000000000000000, 0.000000000000000000, 1.224646799147352961E-16 ) ) ;
#3139 = AXIS2_PLACEMENT_3D ( 'NONE', #6934, #1228, #555 ) ;
#3140 = EDGE_CURVE ( 'NONE', #9216, #6035, #8863, .T. ) ;
#3141 = LINE ( 'NONE', #10259, #10184 ) ;
#3142 = VERTEX_POINT ( 'NONE', #2073 ) ;
#3143 = DIRECTION ( 'NONE',  ( 0.000000000000000000, 0.000000000000000000, 1.000000000000000000 ) ) ;
#3144 = CARTESIAN_POINT ( 'NONE',  ( -27.43301270000000969, 4.799999998907525267, 11.36312591709335784 ) ) ;
#3145 = ORIENTED_EDGE ( 'NONE', *, *, #3853, .F. ) ;
#3146 = APPLICATION_CONTEXT ( 'automotive_design' ) ;
#3147 = CARTESIAN_POINT ( 'NONE',  ( -2.499999999999999556, -4.462499999999999467, 1.443375672974065882 ) ) ;
#3148 = MECHANICAL_DESIGN_GEOMETRIC_PRESENTATION_REPRESENTATION (  '', ( #453 ), #7146 ) ;
#3149 = PRODUCT_DEFINITION ( 'UNKNOWN', '', #5131, #9255 ) ;
#3150 = ADVANCED_BREP_SHAPE_REPRESENTATION ( '', ( #6259, #5055 ), #738 ) ;
#3151 = CARTESIAN_POINT ( 'NONE',  ( -20.91430522584054330, 100.0000000000000142, -10.19152558580213608 ) ) ;
#3152 = CARTESIAN_POINT ( 'NONE',  ( 2.256430356250000102, -4.078124999385482674, -2.763330213280484622E-16 ) ) ;
#3153 = EDGE_CURVE ( 'NONE', #2830, #5524, #5268, .T. ) ;
#3154 = CARTESIAN_POINT ( 'NONE',  ( -20.89884294283097432, 99.50000000000001421, -10.47119744953613640 ) ) ;
#3155 = CARTESIAN_POINT ( 'NONE',  ( 27.00000000000000355, 1.449999997815050401, -11.18376618407356737 ) ) ;
#3156 = CARTESIAN_POINT ( 'NONE',  ( -15.10687288066601930, 99.49999999999998579, 15.84109048427130517 ) ) ;
#3157 = CARTESIAN_POINT ( 'NONE',  ( 3.478562133589548910, 99.99999999999997158, -24.13114810667639532 ) ) ;
#3158 = CARTESIAN_POINT ( 'NONE',  ( 3.214822648120007731, 99.50000000000000000, -21.86319392453323829 ) ) ;
#3159 = AXIS2_PLACEMENT_3D ( 'NONE', #5347, #8424, #1472 ) ;
#3160 = CARTESIAN_POINT ( 'NONE',  ( 1.128215178125001161, -3.140624999385482674, 1.954126010382870815 ) ) ;
#3161 = CARTESIAN_POINT ( 'NONE',  ( 4.034460619503033030, 99.99999999999995737, -21.08676866017170681 ) ) ;
#3162 = CARTESIAN_POINT ( 'NONE',  ( -1.128215178124998497, -3.215624999385482408, 1.954126010382872147 ) ) ;
#3163 = CARTESIAN_POINT ( 'NONE',  ( -11.36312591709337383, 4.799999998907525267, 27.43301269999999548 ) ) ;
#3164 =( NAMED_UNIT ( * ) PLANE_ANGLE_UNIT ( ) SI_UNIT ( $, .RADIAN. ) );
#3165 = CARTESIAN_POINT ( 'NONE',  ( 4.154273145530666511, 99.50000000000000000, -22.82723029927519676 ) ) ;
#3166 = CARTESIAN_POINT ( 'NONE',  ( -27.00000000000000355, 2.799999999999999822, -3.306546357697854128E-15 ) ) ;
#3167 = VECTOR ( 'NONE', #8931, 1000.000000000000000 ) ;
#3168 = CARTESIAN_POINT ( 'NONE',  ( 0.000000000000000000, -5.000000000000000000, 0.000000000000000000 ) ) ;
#3169 = CARTESIAN_POINT ( 'NONE',  ( 8.081885929396888102, 100.0000000000000142, 20.89785832093561169 ) ) ;
#3170 = VERTEX_POINT ( 'NONE', #10067 ) ;
#3171 = VERTEX_POINT ( 'NONE', #494 ) ;
#3172 = CARTESIAN_POINT ( 'NONE',  ( 1.128215178124999607, -4.453124999385482674, -1.954126010382871259 ) ) ;
#3173 = FACE_OUTER_BOUND ( 'NONE', #8422, .T. ) ;
#3174 = CARTESIAN_POINT ( 'NONE',  ( 19.39806930854668110, 1.149999998907525356, -19.39806930854668110 ) ) ;
#3175 = CARTESIAN_POINT ( 'NONE',  ( 3.238942592553923472, 100.0000000000000142, -24.36085717291697250 ) ) ;
#3176 = CARTESIAN_POINT ( 'NONE',  ( -22.51488550592518934, 99.49999999999997158, -10.97145172607810615 ) ) ;
#3177 = CARTESIAN_POINT ( 'NONE',  ( -1.128215178124998497, -3.778124999385482408, 1.954126010382872147 ) ) ;
#3178 = CARTESIAN_POINT ( 'NONE',  ( 0.000000000000000000, 100.0000000000000000, -27.00000000000000355 ) ) ;
#3179 = CARTESIAN_POINT ( 'NONE',  ( 9.802580223201115217, 99.99999999999995737, 21.25247094773282086 ) ) ;
#3180 = DIRECTION ( 'NONE',  ( 0.000000000000000000, 1.000000000000000000, 0.000000000000000000 ) ) ;
#3181 = CARTESIAN_POINT ( 'NONE',  ( 2.500000000000000444, -1.556249998770965925, 1.443375672974063439 ) ) ;
#3182 = CARTESIAN_POINT ( 'NONE',  ( 10.85214315541671759, 99.50000000000000000, 22.51047735782115211 ) ) ;
#3183 = DIRECTION ( 'NONE',  ( -0.000000000000000000, -1.000000000000000000, -0.000000000000000000 ) ) ;
#3184 = CARTESIAN_POINT ( 'NONE',  ( -2.500000000000000000, -4.481249998770965526, -1.443375672974064106 ) ) ;
#3185 =( BOUNDED_CURVE ( )  B_SPLINE_CURVE ( 2, ( #1275, #4633, #6088, #2054, #7036, #1385, #7826, #602, #2110 ),
 .UNSPECIFIED., .F., .T. ) 
 B_SPLINE_CURVE_WITH_KNOTS ( ( 3, 2, 2, 2, 3 ),
 ( 0.02083333333333333565, 0.02777777777777777624, 0.04166666666666666435, 0.05555555555555555247, 0.06250000000000000000 ),
 .UNSPECIFIED. ) 
 CURVE ( )  GEOMETRIC_REPRESENTATION_ITEM ( )  RATIONAL_B_SPLINE_CURVE ( ( 0.9330127018922194093, 0.9330127018922194093, 1.000000000000000000, 0.8660254037844387076, 1.000000000000000000, 0.8660254037844387076, 1.000000000000000000, 0.9330127018922194093, 0.9330127018922194093 ) ) 
 REPRESENTATION_ITEM ( '' )  );
#3186 = CARTESIAN_POINT ( 'NONE',  ( -2.256430356250000102, -2.878124999385482941, -1.302750673588580321 ) ) ;
#3187 = EDGE_CURVE ( 'NONE', #9293, #4730, #7657, .T. ) ;
#3188 = PRODUCT_DEFINITION_SHAPE ( 'NONE', 'NONE',  #2372 ) ;
#3189 = EDGE_LOOP ( 'NONE', ( #1395, #3381, #4742, #5806, #2051, #5447, #9134, #947, #3412, #991, #3971, #7508, #1405, #3575, #7924, #5695, #5542, #290, #1220, #31, #692, #9551, #7080, #6301, #9958, #4852 ) ) ;
#3190 = CARTESIAN_POINT ( 'NONE',  ( -22.34867803760930727, 99.99999999999998579, -10.48295844864103721 ) ) ;
#3191 = ORIENTED_EDGE ( 'NONE', *, *, #6377, .T. ) ;
#3192 = CARTESIAN_POINT ( 'NONE',  ( 1.249999999999999334, -1.893749998770965837, -2.165063509461096825 ) ) ;
#3193 = CARTESIAN_POINT ( 'NONE',  ( -14.89508182811745662, 99.49999999999997158, 15.38112983991209326 ) ) ;
#3194 = CARTESIAN_POINT ( 'NONE',  ( -5.039362679103552881E-15, 3.349999998907525534, 27.43301270000000258 ) ) ;
#3195 = ORIENTED_EDGE ( 'NONE', *, *, #6715, .F. ) ;
#3196 = CARTESIAN_POINT ( 'NONE',  ( -1.767625397874844694E-16, -4.162499999999999645, -2.886751345948128655 ) ) ;
#3197 = EDGE_CURVE ( 'NONE', #7555, #4497, #1492, .T. ) ;
#3198 = CARTESIAN_POINT ( 'NONE',  ( 3.282077632710153292, 99.99999999999997158, -23.74569985055724786 ) ) ;
#3199 = CARTESIAN_POINT ( 'NONE',  ( 2.256430356249999658, -3.590624999385481964, -1.302750673588581432 ) ) ;
#3200 = CARTESIAN_POINT ( 'NONE',  ( 0.000000000000000000, 0.000000000000000000, 0.000000000000000000 ) ) ;
#3201 = CARTESIAN_POINT ( 'NONE',  ( 1.679787559701184688E-15, 5.349999998907525089, -27.43301270000000258 ) ) ;
#3202 = CARTESIAN_POINT ( 'NONE',  ( -20.42657152723830905, 99.50000000000000000, -10.54129411626120216 ) ) ;
#3203 = CARTESIAN_POINT ( 'NONE',  ( 3.597125852879613728, 99.99999999999998579, -24.22990373345680126 ) ) ;
#3204 = DIRECTION ( 'NONE',  ( 0.000000000000000000, 0.000000000000000000, -1.000000000000000000 ) ) ;
#3205 = PLANE ( 'NONE',  #5965 ) ;
#3206 = CARTESIAN_POINT ( 'NONE',  ( -1.595409442497313560E-16, -4.303124999385482319, -2.605501347177161087 ) ) ;
#3207 = CARTESIAN_POINT ( 'NONE',  ( 3.861186820804014097, 100.0000000000000426, -21.07288982789904708 ) ) ;
#3208 = VERTEX_POINT ( 'NONE', #6144 ) ;
#3209 = VERTEX_POINT ( 'NONE', #6871 ) ;
#3210 = CARTESIAN_POINT ( 'NONE',  ( -2.256430356249999214, -2.803124999385482763, 1.302750673588581876 ) ) ;
#3211 = CARTESIAN_POINT ( 'NONE',  ( 27.43301270000000258, 1.949999998907525178, 0.000000000000000000 ) ) ;
#3212 = CARTESIAN_POINT ( 'NONE',  ( 6.246869686064662197, 99.50000000000000000, 20.92172973853146090 ) ) ;
#3213 = B_SPLINE_CURVE_WITH_KNOTS ( 'NONE', 3,
 ( #91, #9467, #1558, #2296, #8682, #8782, #10358, #7891, #9567, #5593, #1607 ),
 .UNSPECIFIED., .F., .F.,
 ( 4, 1, 1, 1, 1, 1, 1, 1, 4 ),
 ( 0.000000000000000000, 0.1307887167449866828, 0.2576322083635017579, 0.3824781763252146916, 0.5056045358258490774, 0.6278910088851102911, 0.7502354365656509483, 0.8735741898580190457, 1.000000000000000000 ),
 .UNSPECIFIED. ) ;
#3214 = CARTESIAN_POINT ( 'NONE',  ( 11.36312591709336139, 0.3999999989075253559, -27.43301270000000258 ) ) ;
#3215 = DIRECTION ( 'NONE',  ( 0.000000000000000000, 0.000000000000000000, -1.000000000000000000 ) ) ;
#3216 = SURFACE_SIDE_STYLE ('',( #4098 ) ) ;
#3217 = CARTESIAN_POINT ( 'NONE',  ( -21.24310748994415832, 99.99999999999995737, -10.99527971241054658 ) ) ;
#3218 = CARTESIAN_POINT ( 'NONE',  ( -2.256430356250000102, -3.853124999385482585, 0.000000000000000000 ) ) ;
#3219 = CARTESIAN_POINT ( 'NONE',  ( 11.36312591709336850, 4.099999998907525089, 27.43301269999999903 ) ) ;
#3220 = CARTESIAN_POINT ( 'NONE',  ( -11.18376618407356737, 1.850000000000000311, -27.00000000000000355 ) ) ;
#3221 = VECTOR ( 'NONE', #659, 1000.000000000000000 ) ;
#3222 = ADVANCED_FACE ( 'NONE', ( #8670 ), #7771, .T. ) ;
#3223 = CARTESIAN_POINT ( 'NONE',  ( 1.653273178848927064E-15, 0.7999999978150503788, -27.00000000000000355 ) ) ;
#3224 = CARTESIAN_POINT ( 'NONE',  ( 2.256430356249999658, -4.040624999385483029, -1.302750673588581432 ) ) ;
#3225 = CARTESIAN_POINT ( 'NONE',  ( -19.09188309203678813, 1.899999997815050579, 19.09188309203678457 ) ) ;
#3226 = CARTESIAN_POINT ( 'NONE',  ( -22.64023588676181475, 100.0000000000000000, -10.01165679465830927 ) ) ;
#3227 = CARTESIAN_POINT ( 'NONE',  ( 4.688812652749139609, 100.0000000000000142, -24.54863390154074310 ) ) ;
#3228 = VECTOR ( 'NONE', #7194, 1000.000000000000000 ) ;
#3229 = CARTESIAN_POINT ( 'NONE',  ( -2.500000000000000000, -2.231249998770965970, -1.443375672974064106 ) ) ;
#3230 = EDGE_LOOP ( 'NONE', ( #4585, #8662, #7224, #2517, #2543, #3909, #298, #8196 ) ) ;
#3231 = CARTESIAN_POINT ( 'NONE',  ( 1.250000000000001110, -1.143749998770965837, 2.165063509461096380 ) ) ;
#3232 = CARTESIAN_POINT ( 'NONE',  ( -15.34367147589386349, 100.0000000000000426, 16.87599331055909602 ) ) ;
#3233 = LINE ( 'NONE', #2444, #1373 ) ;
#3234 = CARTESIAN_POINT ( 'NONE',  ( 4.786228327491941173E-16, -4.978124999385483029, 2.605501347177161087 ) ) ;
#3235 = CIRCLE ( 'NONE', #50, 23.99999999999999645 ) ;
#3236 = ORIENTED_EDGE ( 'NONE', *, *, #9066, .F. ) ;
#3237 = CARTESIAN_POINT ( 'NONE',  ( -22.29247428061501779, 100.0000000000000000, -10.66603791136541624 ) ) ;
#3238 = VERTEX_POINT ( 'NONE', #4519 ) ;
#3239 = DIRECTION ( 'NONE',  ( 0.9789429660840185399, 0.000000000000000000, -0.2041339490496966447 ) ) ;
#3240 = CARTESIAN_POINT ( 'NONE',  ( -14.79004890936967875, 99.49999999999998579, 16.19006955939758541 ) ) ;
#3241 = VECTOR ( 'NONE', #2751, 1000.000000000000000 ) ;
#3242 = CARTESIAN_POINT ( 'NONE',  ( 27.43301269999999548, 4.299999998907526155, 11.36312591709337916 ) ) ;
#3243 = ORIENTED_EDGE ( 'NONE', *, *, #5357, .F. ) ;
#3244 = CARTESIAN_POINT ( 'NONE',  ( 4.128176300878408256, 99.50000000000001421, -21.47174600747824869 ) ) ;
#3245 = CARTESIAN_POINT ( 'NONE',  ( -20.89145576992255116, 99.99999999999997158, -10.33073932272468198 ) ) ;
#3246 = CARTESIAN_POINT ( 'NONE',  ( -1.128215178125000273, -4.378124999385482496, -1.954126010382871259 ) ) ;
#3247 = CARTESIAN_POINT ( 'NONE',  ( -20.45905772418405988, 100.0000000000000000, -10.59533404166311321 ) ) ;
#3248 = CARTESIAN_POINT ( 'NONE',  ( 1.653273178848927064E-15, 1.599999997815050312, -27.00000000000000355 ) ) ;
#3249 = CARTESIAN_POINT ( 'NONE',  ( -3.486133158594716510E-16, -1.406249998770965570, -2.500000000000000000 ) ) ;
#3250 = FACE_OUTER_BOUND ( 'NONE', #5456, .T. ) ;
#3251 = CARTESIAN_POINT ( 'NONE',  ( -15.33577160963320374, 99.49999999999998579, 16.45272793336155814 ) ) ;
#3252 = EDGE_CURVE ( 'NONE', #3431, #2986, #8934, .T. ) ;
#3253 = DIRECTION ( 'NONE',  ( -1.000000000000000000, 0.000000000000000000, 0.000000000000000000 ) ) ;
#3254 = CARTESIAN_POINT ( 'NONE',  ( -2.256430356250000102, -4.640624999385482674, 0.000000000000000000 ) ) ;
#3255 = CARTESIAN_POINT ( 'NONE',  ( 9.576498344683301411, 99.99999999999998579, 20.78592410672095880 ) ) ;
#3256 = VERTEX_POINT ( 'NONE', #8560 ) ;
#3257 = ORIENTED_EDGE ( 'NONE', *, *, #7088, .F. ) ;
#3258 = CARTESIAN_POINT ( 'NONE',  ( 1.128215178124999607, -1.640624999385482896, -1.954126010382871259 ) ) ;
#3259 = CARTESIAN_POINT ( 'NONE',  ( 19.39806930854667399, 4.149999998907525800, 19.39806930854668465 ) ) ;
#3260 = CARTESIAN_POINT ( 'NONE',  ( -15.24337324910153946, 99.49999999999997158, 16.81353386054630761 ) ) ;
#3261 = CARTESIAN_POINT ( 'NONE',  ( 26.99999999999999645, 3.150000000000000355, 11.18376618407358691 ) ) ;
#3262 = CARTESIAN_POINT ( 'NONE',  ( 2.500000000000000000, -3.318749998770965437, -3.061616997868383141E-16 ) ) ;
#3263 = CYLINDRICAL_SURFACE ( 'NONE', #4380, 27.00000000000000355 ) ;
#3264 = EDGE_CURVE ( 'NONE', #1900, #9216, #3185, .T. ) ;
#3265 = CARTESIAN_POINT ( 'NONE',  ( 4.750280232731688201, 100.0000000000000284, -24.05275076595185624 ) ) ;
#3266 = ORIENTED_EDGE ( 'NONE', *, *, #7879, .T. ) ;
#3267 = CARTESIAN_POINT ( 'NONE',  ( 27.43301270000000258, 4.249999998907525445, 0.000000000000000000 ) ) ;
#3268 = CARTESIAN_POINT ( 'NONE',  ( 2.940631318607589417, 99.50000000000000000, -23.77584808773673331 ) ) ;
#3269 = B_SPLINE_SURFACE_WITH_KNOTS ( 'NONE', 3, 1, ( 
 ( #5763, #5014 ),
 ( #8951, #8211 ),
 ( #1819, #361 ),
 ( #3395, #1197 ),
 ( #5168, #5904 ),
 ( #8367, #1043 ),
 ( #4389, #4285 ),
 ( #9100, #3551 ),
 ( #9831, #4237 ),
 ( #6740, #2569 ),
 ( #7469, #6587 ),
 ( #7574, #3498 ),
 ( #1868, #2663 ),
 ( #7418, #258 ),
 ( #8264, #8164 ) ),
 .UNSPECIFIED., .F., .F., .F.,
 ( 4, 1, 1, 1, 1, 1, 1, 1, 1, 1, 1, 1, 4 ),
 ( 2, 2 ),
 ( 0.000000000000000000, 0.08490232564366416435, 0.1680779112633816463, 0.2506304657828534177, 0.3338427399641299420, 0.4169763759729993580, 0.4990117930239920674, 0.5811067191809071719, 0.6656374296971073745, 0.7500328835558887075, 0.8331455368193440014, 0.9159638734519762737, 1.000000000000000000 ),
 ( 0.000000000000000000, 1.000000000000000000 ),
 .UNSPECIFIED. ) ;
#3270 = LINE ( 'NONE', #6462, #7245 ) ;
#3271 = CARTESIAN_POINT ( 'NONE',  ( -2.256430356250000102, -4.790624999385483918, -1.302750673588580321 ) ) ;
#3272 = CARTESIAN_POINT ( 'NONE',  ( 2.852289972453743161, 100.0000000000000000, -22.14293542748032451 ) ) ;
#3273 = AXIS2_PLACEMENT_3D ( 'NONE', #3607, #1921, #6791 ) ;
#3274 = CARTESIAN_POINT ( 'NONE',  ( -22.64023588676181475, 99.50000000000000000, -10.01165679465830927 ) ) ;
#3275 = CARTESIAN_POINT ( 'NONE',  ( -4.959819536546781389E-15, 2.200000000000000178, 27.00000000000000355 ) ) ;
#3276 = EDGE_CURVE ( 'NONE', #1380, #3621, #3799, .T. ) ;
#3277 = EDGE_CURVE ( 'NONE', #4882, #1444, #234, .T. ) ;
#3278 = CARTESIAN_POINT ( 'NONE',  ( -1.767625397874844694E-16, -4.556249998770965703, -2.886751345948128655 ) ) ;
#3279 = ORIENTED_EDGE ( 'NONE', *, *, #6211, .F. ) ;
#3280 = CIRCLE ( 'NONE', #9774, 1.324999999999999734 ) ;
#3281 = CARTESIAN_POINT ( 'NONE',  ( 0.6698729810778069060, -0.9763461882033002137, -2.500000000000000000 ) ) ;
#3282 = CARTESIAN_POINT ( 'NONE',  ( -15.34367147589386349, 99.50000000000004263, 16.87599331055909602 ) ) ;
#3283 = CARTESIAN_POINT ( 'NONE',  ( -14.76042637754942177, 100.0000000000000000, 16.05242888258284140 ) ) ;
#3284 = CARTESIAN_POINT ( 'NONE',  ( -2.256430356250000102, -2.840624999385482852, 0.000000000000000000 ) ) ;
#3285 = CARTESIAN_POINT ( 'NONE',  ( -22.35642768247353729, 99.99999999999995737, -10.34293228154892752 ) ) ;
#3286 = VERTEX_POINT ( 'NONE', #7087 ) ;
#3287 = CARTESIAN_POINT ( 'NONE',  ( 0.6698729810778075722, -1.667403810567665623, 2.499999999999999556 ) ) ;
#3288 = CARTESIAN_POINT ( 'NONE',  ( -4.959819536546781389E-15, 2.799999997815050268, 27.00000000000000355 ) ) ;
#3289 = CARTESIAN_POINT ( 'NONE',  ( 8.829292973371666520, 99.99999999999998579, 19.92220432019063736 ) ) ;
#3290 = EDGE_LOOP ( 'NONE', ( #8808, #1408, #3740, #2217 ) ) ;
#3291 =( NAMED_UNIT ( * ) SI_UNIT ( $, .STERADIAN. ) SOLID_ANGLE_UNIT ( ) );
#3292 = CARTESIAN_POINT ( 'NONE',  ( 21.43339342948717885, 100.0000000000000000, -1.392427884615384803 ) ) ;
#3293 = CARTESIAN_POINT ( 'NONE',  ( 2.256430356250000102, -3.628124999385482496, -2.763330213280484622E-16 ) ) ;
#3294 = FACE_OUTER_BOUND ( 'NONE', #6918, .T. ) ;
#3295 = CARTESIAN_POINT ( 'NONE',  ( 27.43301270000000258, 5.199999998907525622, -11.36312591709336139 ) ) ;
#3296 = UNCERTAINTY_MEASURE_WITH_UNIT (LENGTH_MEASURE( 1.000000000000000082E-05 ), #7429, 'distance_accuracy_value', 'NONE');
#3297 = CARTESIAN_POINT ( 'NONE',  ( -15.18657300206754179, 99.50000000000000000, 16.26161032743331347 ) ) ;
#3298 = AXIS2_PLACEMENT_3D ( 'NONE', #7909, #7962, #9582 ) ;
#3299 = CARTESIAN_POINT ( 'NONE',  ( -21.91899880027261460, 99.50000000000000000, -9.705014769524845875 ) ) ;
#3300 = CARTESIAN_POINT ( 'NONE',  ( 3.282077632710153292, 100.0000000000000000, -23.74569985055724786 ) ) ;
#3301 = CARTESIAN_POINT ( 'NONE',  ( -22.33111803333905243, 99.99999999999997158, -9.558150950182401573 ) ) ;
#3302 = CARTESIAN_POINT ( 'NONE',  ( -1.595409442497313560E-16, -2.953124999385483118, -2.605501347177161087 ) ) ;
#3303 = CARTESIAN_POINT ( 'NONE',  ( 3.810791133452845703, 99.50000000000005684, -24.33305202239136733 ) ) ;
#3304 = ORIENTED_EDGE ( 'NONE', *, *, #3430, .F. ) ;
#3305 = CARTESIAN_POINT ( 'NONE',  ( -2.256430356250000102, -3.740624999385482763, 0.000000000000000000 ) ) ;
#3306 = CARTESIAN_POINT ( 'NONE',  ( -27.43301270000000258, 4.649999998907525800, -3.359575119402369376E-15 ) ) ;
#3307 = EDGE_CURVE ( 'NONE', #6092, #3729, #3021, .T. ) ;
#3308 = LINE ( 'NONE', #2367, #10118 ) ;
#3309 = EDGE_CURVE ( 'NONE', #3016, #7000, #9395, .T. ) ;
#3310 = CARTESIAN_POINT ( 'NONE',  ( 19.09188309203678813, 4.100000000000000533, -19.09188309203678813 ) ) ;
#3311 = CARTESIAN_POINT ( 'NONE',  ( -20.70854316912038229, 100.0000000000000142, -10.95957977981033515 ) ) ;
#3312 = DIRECTION ( 'NONE',  ( 0.000000000000000000, 0.000000000000000000, 1.000000000000000000 ) ) ;
#3313 = CARTESIAN_POINT ( 'NONE',  ( -21.24310748994415832, 99.49999999999998579, -10.99527971241054658 ) ) ;
#3314 = CARTESIAN_POINT ( 'NONE',  ( -20.77412980915959650, 99.99999999999991473, -9.759484723497815040 ) ) ;
#3315 = CARTESIAN_POINT ( 'NONE',  ( -11.36312591709337561, 4.799999998907525267, 27.43301269999999548 ) ) ;
#3316 = CARTESIAN_POINT ( 'NONE',  ( 3.606694021351891877, 99.50000000000000000, -24.61315535935035115 ) ) ;
#3317 = CARTESIAN_POINT ( 'NONE',  ( -21.98271324694694329, 99.50000000000000000, -11.39207625356720222 ) ) ;
#3318 = VECTOR ( 'NONE', #2310, 1000.000000000000114 ) ;
#3319 = CARTESIAN_POINT ( 'NONE',  ( 2.256430356250000546, -3.215624999385482408, 1.302750673588579877 ) ) ;
#3320 = CARTESIAN_POINT ( 'NONE',  ( -16.57687742313193269, 100.0000000000000284, 15.91855687263828756 ) ) ;
#3321 = EDGE_CURVE ( 'NONE', #1380, #9254, #641, .T. ) ;
#3322 = CARTESIAN_POINT ( 'NONE',  ( 11.18376618407357626, 1.450000000000000400, 27.00000000000000000 ) ) ;
#3323 = CARTESIAN_POINT ( 'NONE',  ( 1.034219503716432668E-14, -4.612500000000000711, -2.500000000000000000 ) ) ;
#3324 = CARTESIAN_POINT ( 'NONE',  ( 2.500000000000000000, -3.768749998770965171, -3.061616997868383141E-16 ) ) ;
#3325 = ORIENTED_EDGE ( 'NONE', *, *, #2860, .F. ) ;
#3326 = CARTESIAN_POINT ( 'NONE',  ( -21.56977948371741505, 99.99999999999995737, -11.44450812306045329 ) ) ;
#3327 = DIRECTION ( 'NONE',  ( 0.000000000000000000, 0.000000000000000000, 1.000000000000000000 ) ) ;
#3328 =( BOUNDED_CURVE ( )  B_SPLINE_CURVE ( 2, ( #1663, #4857, #2503, #3528, #6615, #1122, #3422, #1751, #4994 ),
 .UNSPECIFIED., .F., .F. ) 
 B_SPLINE_CURVE_WITH_KNOTS ( ( 3, 2, 2, 2, 3 ),
 ( 0.6458333333333333703, 0.6527777777777777901, 0.6666666666666666297, 0.6805555555555555802, 0.6875000000000000000 ),
 .UNSPECIFIED. ) 
 CURVE ( )  GEOMETRIC_REPRESENTATION_ITEM ( )  RATIONAL_B_SPLINE_CURVE ( ( 0.9330127018922192983, 0.9330127018922198534, 1.000000000000000000, 0.8660254037844387076, 1.000000000000000000, 0.8660254037844387076, 1.000000000000000000, 0.9330127018922194093, 0.9330127018922194093 ) ) 
 REPRESENTATION_ITEM ( '' )  );
#3329 = EDGE_CURVE ( 'NONE', #9169, #9715, #864, .T. ) ;
#3330 = CARTESIAN_POINT ( 'NONE',  ( -19.75840245672548789, 99.50000000000000000, -8.735905494466331689 ) ) ;
#3331 = CARTESIAN_POINT ( 'NONE',  ( -1.595409442497313560E-16, -3.853124999385482585, -2.605501347177161087 ) ) ;
#3332 = CARTESIAN_POINT ( 'NONE',  ( 8.074269155311188939, 99.50000000000001421, 20.56111086218762551 ) ) ;
#3333 = CARTESIAN_POINT ( 'NONE',  ( 0.000000000000000000, 70.00000000000000000, 23.99999999999999645 ) ) ;
#3334 = CARTESIAN_POINT ( 'NONE',  ( -4.959819536546781389E-15, 1.199999997815050401, 27.00000000000000355 ) ) ;
#3335 = CARTESIAN_POINT ( 'NONE',  ( -27.00000000000000355, 4.400000000000000355, -3.306546357697854128E-15 ) ) ;
#3336 = VERTEX_POINT ( 'NONE', #2485 ) ;
#3337 = EDGE_CURVE ( 'NONE', #7747, #7847, #3235, .T. ) ;
#3338 = CARTESIAN_POINT ( 'NONE',  ( -2.499999999999999112, -4.462499999999999467, 1.443375672974065882 ) ) ;
#3339 = CARTESIAN_POINT ( 'NONE',  ( 7.812290123947159159, 99.99999999999994316, 21.17203503082402349 ) ) ;
#3340 = CARTESIAN_POINT ( 'NONE',  ( -20.97746206809550884, 99.50000000000000000, -11.22189255051946688 ) ) ;
#3341 = CARTESIAN_POINT ( 'NONE',  ( 27.00000000000000355, 0.6499999978150502455, -11.18376618407356737 ) ) ;
#3342 = FACE_OUTER_BOUND ( 'NONE', #5022, .T. ) ;
#3343 = CARTESIAN_POINT ( 'NONE',  ( 2.500000000000000000, -4.668749998770964638, -3.061616997868383141E-16 ) ) ;
#3344 = CARTESIAN_POINT ( 'NONE',  ( -15.62070810370258833, 99.50000000000000000, 16.62245103965875970 ) ) ;
#3345 = CARTESIAN_POINT ( 'NONE',  ( 27.43301270000000258, 0.2499999989075252504, 0.000000000000000000 ) ) ;
#3346 = CARTESIAN_POINT ( 'NONE',  ( 9.877377282685029372E-16, -4.781249998770965348, 2.500000000000000000 ) ) ;
#3347 = ORIENTED_EDGE ( 'NONE', *, *, #1218, .T. ) ;
#3348 = ORIENTED_EDGE ( 'NONE', *, *, #5765, .T. ) ;
#3349 = CARTESIAN_POINT ( 'NONE',  ( -1.595409442497313560E-16, -4.303124999385482319, -2.605501347177161087 ) ) ;
#3350 = FILL_AREA_STYLE ('',( #5808 ) ) ;
#3351 = CARTESIAN_POINT ( 'NONE',  ( 0.000000000000000000, 0.000000000000000000, 0.000000000000000000 ) ) ;
#3352 = CARTESIAN_POINT ( 'NONE',  ( 19.09188309203678102, 3.900000000000000355, 19.09188309203678813 ) ) ;
#3353 = CARTESIAN_POINT ( 'NONE',  ( 0.6698729810778075722, -3.411153809338631326, 2.499999999999999556 ) ) ;
#3354 = CARTESIAN_POINT ( 'NONE',  ( -2.499999999999999112, -1.312499999999999778, 1.443375672974065882 ) ) ;
#3355 = CARTESIAN_POINT ( 'NONE',  ( -9.703070624755296135E-15, -3.487499999999999822, 2.500000000000000444 ) ) ;
#3356 = CARTESIAN_POINT ( 'NONE',  ( -20.89884294283097432, 99.99999999999998579, -10.47119744953613640 ) ) ;
#3357 = EDGE_CURVE ( 'NONE', #1485, #7448, #1303, .T. ) ;
#3358 = CARTESIAN_POINT ( 'NONE',  ( 19.09188309203678813, 0.1000000000000000056, -19.09188309203678813 ) ) ;
#3359 = LINE ( 'NONE', #7288, #10143 ) ;
#3360 = CARTESIAN_POINT ( 'NONE',  ( 2.971063225226878046, 99.50000000000000000, -23.91837856253154015 ) ) ;
#3361 = CARTESIAN_POINT ( 'NONE',  ( 2.256430356250000546, -4.115624999385482319, 1.302750673588579877 ) ) ;
#3362 = CARTESIAN_POINT ( 'NONE',  ( -22.63784607493503387, 99.50000000000001421, -10.71517552924587058 ) ) ;
#3363 = CARTESIAN_POINT ( 'NONE',  ( -22.58826642033182353, 99.99999999999998579, -9.883148377786627137 ) ) ;
#3364 = CARTESIAN_POINT ( 'NONE',  ( 8.281567445270807681, 100.0000000000000000, 20.15885744430370252 ) ) ;
#3365 = CARTESIAN_POINT ( 'NONE',  ( -2.500000000000000000, -4.931249998770966592, -1.443375672974064106 ) ) ;
#3366 = VERTEX_POINT ( 'NONE', #8816 ) ;
#3367 = ADVANCED_FACE ( 'NONE', ( #76 ), #4851, .T. ) ;
#3368 = FACE_OUTER_BOUND ( 'NONE', #5665, .T. ) ;
#3369 = CARTESIAN_POINT ( 'NONE',  ( 3.717146347979291665, 99.50000000000000000, -21.42716062222556417 ) ) ;
#3370 = CARTESIAN_POINT ( 'NONE',  ( 9.666415885916139317, 99.50000000000001421, 19.95264712196244261 ) ) ;
#3371 = CARTESIAN_POINT ( 'NONE',  ( -2.256430356250000102, -3.328124999385483562, -1.302750673588580321 ) ) ;
#3372 = VERTEX_POINT ( 'NONE', #5972 ) ;
#3373 = CIRCLE ( 'NONE', #7726, 1.324999999999999734 ) ;
#3374 = FACE_OUTER_BOUND ( 'NONE', #2323, .T. ) ;
#3375 = SHAPE_REPRESENTATION ( 'MAS-199', ( #2798, #9150, #8480, #9499, #134, #5307, #9657, #8824 ), #3978 ) ;
#3376 = LINE ( 'NONE', #6716, #8841 ) ;
#3377 = CARTESIAN_POINT ( 'NONE',  ( -22.24883010645271852, 99.99999999999997158, -10.75389422444101939 ) ) ;
#3378 = CARTESIAN_POINT ( 'NONE',  ( 3.207968951880266761, 99.99999999999998579, -22.92616835434091627 ) ) ;
#3379 = CARTESIAN_POINT ( 'NONE',  ( 3.635130212803377781, 99.50000000000000000, -23.00575896550913768 ) ) ;
#3380 = CARTESIAN_POINT ( 'NONE',  ( 8.393217272293057363, 99.99999999999994316, 19.69436072183531650 ) ) ;
#3381 = ORIENTED_EDGE ( 'NONE', *, *, #3951, .T. ) ;
#3382 = DIRECTION ( 'NONE',  ( 0.000000000000000000, -0.000000000000000000, -1.000000000000000000 ) ) ;
#3383 = CARTESIAN_POINT ( 'NONE',  ( 27.00000000000000355, 3.799999997815050268, 0.000000000000000000 ) ) ;
#3384 = EDGE_CURVE ( 'NONE', #9410, #8654, #2191, .T. ) ;
#3385 = DIRECTION ( 'NONE',  ( -0.000000000000000000, -1.000000000000000000, 0.000000000000000000 ) ) ;
#3386 = AXIS2_PLACEMENT_3D ( 'NONE', #4735, #4838, #4785 ) ;
#3387 = CARTESIAN_POINT ( 'NONE',  ( -21.38163724633288965, 99.50000000000005684, -9.681902434707239991 ) ) ;
#3388 = CARTESIAN_POINT ( 'NONE',  ( 8.685676809262872666, 99.50000000000000000, 23.43455588346217766 ) ) ;
#3389 = EDGE_CURVE ( 'NONE', #647, #7345, #9931, .T. ) ;
#3390 = CARTESIAN_POINT ( 'NONE',  ( -21.33175168474226879, 100.0000000000000142, -11.03889704119913162 ) ) ;
#3391 = DIRECTION ( 'NONE',  ( -0.9804671828129908340, 0.000000000000000000, 0.1966827481675937628 ) ) ;
#3392 = EDGE_LOOP ( 'NONE', ( #8665, #3039, #9271, #2337 ) ) ;
#3393 = ORIENTED_EDGE ( 'NONE', *, *, #3520, .T. ) ;
#3394 = CARTESIAN_POINT ( 'NONE',  ( -1.128215178125000273, -4.265624999385482674, -1.954126010382871259 ) ) ;
#3395 = CARTESIAN_POINT ( 'NONE',  ( -14.89508182811745662, 99.49999999999997158, 15.38112983991209326 ) ) ;
#3396 = CARTESIAN_POINT ( 'NONE',  ( 21.79306891025641235, 99.50000000000000000, -1.065004006410256387 ) ) ;
#3397 = CARTESIAN_POINT ( 'NONE',  ( -27.43301270000000258, 3.799999998907525711, -11.36312591709336317 ) ) ;
#3398 = CYLINDRICAL_SURFACE ( 'NONE', #2090, 17.50000000000000355 ) ;
#3399 = DIRECTION ( 'NONE',  ( 0.000000000000000000, 1.000000000000000000, 0.000000000000000000 ) ) ;
#3400 = LINE ( 'NONE', #9593, #4895 ) ;
#3401 = ORIENTED_EDGE ( 'NONE', *, *, #592, .T. ) ;
#3402 = EDGE_LOOP ( 'NONE', ( #9393, #9356 ) ) ;
#3403 = CARTESIAN_POINT ( 'NONE',  ( -21.49703851962343037, 99.49999999999997158, -9.300281078773625865 ) ) ;
#3404 = CARTESIAN_POINT ( 'NONE',  ( -19.39806930854667755, 4.549999998907525267, -19.39806930854668110 ) ) ;
#3405 = CARTESIAN_POINT ( 'NONE',  ( 9.526713201929464248, 99.50000000000000000, 20.38668308130821671 ) ) ;
#3406 = CARTESIAN_POINT ( 'NONE',  ( -16.25490828497592588, 99.49999999999998579, 14.91257814242970348 ) ) ;
#3407 = CARTESIAN_POINT ( 'NONE',  ( -16.33590634957226229, 100.0000000000000000, 16.80570853669505382 ) ) ;
#3408 = CARTESIAN_POINT ( 'NONE',  ( 27.00000000000000355, 1.649999999999999911, -11.18376618407356915 ) ) ;
#3409 = CARTESIAN_POINT ( 'NONE',  ( 8.515772100368442565, 100.0000000000000000, 20.00046577258137503 ) ) ;
#3410 = EDGE_LOOP ( 'NONE', ( #7734, #810, #6127 ) ) ;
#3411 = CARTESIAN_POINT ( 'NONE',  ( 1.128215178124999607, -0.4031249993854829627, -1.954126010382871259 ) ) ;
#3412 = ORIENTED_EDGE ( 'NONE', *, *, #3321, .F. ) ;
#3413 = ORIENTED_EDGE ( 'NONE', *, *, #9332, .T. ) ;
#3414 = CARTESIAN_POINT ( 'NONE',  ( 0.000000000000000000, 100.0000000000000000, -27.00000000000000355 ) ) ;
#3415 = CARTESIAN_POINT ( 'NONE',  ( 3.207057600658871355, 99.50000000000000000, -22.07913334414698880 ) ) ;
#3416 = AXIS2_PLACEMENT_3D ( 'NONE', #1302, #679, #5397 ) ;
#3417 = CARTESIAN_POINT ( 'NONE',  ( -21.33175168474226879, 99.50000000000001421, -11.03889704119913162 ) ) ;
#3418 = DIRECTION ( 'NONE',  ( -1.224646799147353207E-16, 1.000000000000000000, 0.000000000000000000 ) ) ;
#3419 = EDGE_CURVE ( 'NONE', #4212, #7890, #9010, .T. ) ;
#3420 = CIRCLE ( 'NONE', #1091, 7.500000000000000000 ) ;
#3421 = LINE ( 'NONE', #6478, #4952 ) ;
#3422 = CARTESIAN_POINT ( 'NONE',  ( -1.250000000000000222, -3.674999999999999822, -2.165063509461096825 ) ) ;
#3423 = DIRECTION ( 'NONE',  ( -0.9961946980917455452, -0.08715574274765837404, 0.000000000000000000 ) ) ;
#3424 = AXIS2_PLACEMENT_3D ( 'NONE', #5871, #2734, #8332 ) ;
#3425 = ORIENTED_EDGE ( 'NONE', *, *, #9123, .F. ) ;
#3426 = B_SPLINE_CURVE_WITH_KNOTS ( 'NONE', 3,
 ( #1413, #6956, #8591, #2407, #4758, #9627, #1671, #3154, #938, #7956, #5603, #789, #2459, #3981, #10316, #6337, #890, #47, #7167 ),
 .UNSPECIFIED., .F., .F.,
 ( 4, 1, 1, 1, 1, 1, 1, 1, 1, 1, 1, 1, 1, 1, 1, 1, 4 ),
 ( 0.000000000000000000, 0.06455295689170470474, 0.1273249605695649933, 0.1891299628201091876, 0.2499617887110622549, 0.3104215510145779122, 0.3717966107350694216, 0.4346754705585744727, 0.4991966429079077727, 0.5636107885140392293, 0.6264421791528413941, 0.6882713145562978641, 0.7491215306807221808, 0.8100115732567139126, 0.8716292230916812267, 0.9349778748807419104, 1.000000000000000000 ),
 .UNSPECIFIED. ) ;
#3427 = DIRECTION ( 'NONE',  ( -0.3368610894541371747, 0.000000000000000000, 0.9415543565890243105 ) ) ;
#3428 = CARTESIAN_POINT ( 'NONE',  ( 4.295198626299898237, 99.50000000000001421, -24.68029520312135361 ) ) ;
#3429 = CARTESIAN_POINT ( 'NONE',  ( 7.729958523985794194, 99.50000000000001421, 20.63140804260154937 ) ) ;
#3430 = EDGE_CURVE ( 'NONE', #2896, #6863, #4348, .T. ) ;
#3431 = VERTEX_POINT ( 'NONE', #1782 ) ;
#3432 = CARTESIAN_POINT ( 'NONE',  ( 9.838488147574068421, 99.50000000000000000, 20.25735696016189280 ) ) ;
#3433 = CARTESIAN_POINT ( 'NONE',  ( -19.09188309203678813, 3.499999997815050445, 19.09188309203678457 ) ) ;
#3434 =( BOUNDED_CURVE ( )  B_SPLINE_CURVE ( 2, ( #7520, #3446, #5809, #311, #2716, #7369, #1971, #9000, #6635 ),
 .UNSPECIFIED., .F., .F. ) 
 B_SPLINE_CURVE_WITH_KNOTS ( ( 3, 2, 2, 2, 3 ),
 ( 0.4791666666666666852, 0.4861111111111111049, 0.5000000000000000000, 0.5138888888888888395, 0.5208333333333333703 ),
 .UNSPECIFIED. ) 
 CURVE ( )  GEOMETRIC_REPRESENTATION_ITEM ( )  RATIONAL_B_SPLINE_CURVE ( ( 0.9330127018922194093, 0.9330127018922196314, 1.000000000000000000, 0.8660254037844387076, 1.000000000000000000, 0.8660254037844387076, 1.000000000000000000, 0.9330127018922187432, 0.9330127018922192983 ) ) 
 REPRESENTATION_ITEM ( '' )  );
#3435 = CARTESIAN_POINT ( 'NONE',  ( -20.71654887124055122, 99.50000000000001421, -9.874326132881018125 ) ) ;
#3436 = CARTESIAN_POINT ( 'NONE',  ( -20.96643530928959720, 100.0000000000000142, -10.05541671241505064 ) ) ;
#3437 = SURFACE_STYLE_FILL_AREA ( #9983 ) ;
#3438 = CARTESIAN_POINT ( 'NONE',  ( -22.28244091826395135, 99.50000000000000000, -10.68852969318427881 ) ) ;
#3439 = CARTESIAN_POINT ( 'NONE',  ( 4.871887406949175769, 99.99999999999995737, -23.77896509604281405 ) ) ;
#3440 = CARTESIAN_POINT ( 'NONE',  ( 2.500000000000000000, -4.687500000000000000, -1.443375672974065438 ) ) ;
#3441 = CIRCLE ( 'NONE', #4449, 2.500000000000000000 ) ;
#3442 = PRODUCT_DEFINITION ( 'UNKNOWN', '', #8308, #3103 ) ;
#3443 = CARTESIAN_POINT ( 'NONE',  ( -1.767625397874844694E-16, -0.1124999999999999889, -2.886751345948128655 ) ) ;
#3444 = ADVANCED_FACE ( 'NONE', ( #5915 ), #7428, .T. ) ;
#3445 =( NAMED_UNIT ( * ) SI_UNIT ( $, .STERADIAN. ) SOLID_ANGLE_UNIT ( ) );
#3446 = CARTESIAN_POINT ( 'NONE',  ( -0.6698729810778081273, -2.607596189432333844, 2.499999999999999112 ) ) ;
#3447 = CARTESIAN_POINT ( 'NONE',  ( 3.058419780146050648, 100.0000000000000000, -23.12871267107006545 ) ) ;
#3448 = CARTESIAN_POINT ( 'NONE',  ( -27.43301270000000969, 3.099999998907525089, 11.36312591709335429 ) ) ;
#3449 = ADVANCED_FACE ( 'NONE', ( #5180 ), #8733, .T. ) ;
#3450 = CARTESIAN_POINT ( 'NONE',  ( 9.676361905416721143, 100.0000000000000142, 21.63547735782115566 ) ) ;
#3451 = TOROIDAL_SURFACE ( 'NONE', #9300, 23.82500000000000284, 1.324999999999999956 ) ;
#3452 = CARTESIAN_POINT ( 'NONE',  ( -21.16695614262292580, 99.50000000000000000, -11.33496398805607441 ) ) ;
#3453 = AXIS2_PLACEMENT_3D ( 'NONE', #4025, #781, #3143 ) ;
#3454 = CYLINDRICAL_SURFACE ( 'NONE', #1793, 27.00000000000000355 ) ;
#3455 = CARTESIAN_POINT ( 'NONE',  ( 8.429066232339796017, 100.0000000000000000, 19.67794530653910101 ) ) ;
#3456 = ADVANCED_FACE ( 'NONE', ( #4297 ), #5719, .F. ) ;
#3457 = EDGE_LOOP ( 'NONE', ( #9362, #5000, #7737, #2440 ) ) ;
#3458 = CARTESIAN_POINT ( 'NONE',  ( -21.69499712064247277, 99.99999999999992895, -9.295461156691713356 ) ) ;
#3459 = CARTESIAN_POINT ( 'NONE',  ( 3.977571997893210032, 100.0000000000000000, -24.70179182097838932 ) ) ;
#3460 = CARTESIAN_POINT ( 'NONE',  ( 0.000000000000000000, -20.00000000000000000, 0.000000000000000000 ) ) ;
#3461 = CARTESIAN_POINT ( 'NONE',  ( -21.20999280589743918, 99.50000000000002842, -11.35389291771566000 ) ) ;
#3462 = CARTESIAN_POINT ( 'NONE',  ( -1.250000000000000222, -1.818749998770965881, -2.165063509461096825 ) ) ;
#3463 = CARTESIAN_POINT ( 'NONE',  ( 11.18376618407357626, 1.249999997815050445, 27.00000000000000000 ) ) ;
#3464 = CARTESIAN_POINT ( 'NONE',  ( 8.757234875838378230, 99.50000000000000000, 19.92790116963689329 ) ) ;
#3465 = EDGE_CURVE ( 'NONE', #3621, #2231, #1022, .T. ) ;
#3466 = CARTESIAN_POINT ( 'NONE',  ( 9.576498344683301411, 99.49999999999998579, 20.78592410672095880 ) ) ;
#3467 = DIRECTION ( 'NONE',  ( -0.000000000000000000, -1.000000000000000000, -0.000000000000000000 ) ) ;
#3468 = ORIENTED_EDGE ( 'NONE', *, *, #8100, .F. ) ;
#3469 = EDGE_CURVE ( 'NONE', #6584, #1392, #4586, .T. ) ;
#3470 = CARTESIAN_POINT ( 'NONE',  ( 1.128215178125001161, -0.5531249993854828739, 1.954126010382870815 ) ) ;
#3471 = ORIENTED_EDGE ( 'NONE', *, *, #9811, .T. ) ;
#3472 = AXIS2_PLACEMENT_3D ( 'NONE', #4049, #6401, #8078 ) ;
#3473 = LINE ( 'NONE', #1745, #6303 ) ;
#3474 = LINE ( 'NONE', #281, #122 ) ;
#3475 = CARTESIAN_POINT ( 'NONE',  ( -15.07178375341841559, 100.0000000000000142, 15.16157792772069968 ) ) ;
#3476 = CARTESIAN_POINT ( 'NONE',  ( 4.295198626299897349, 100.0000000000000284, -24.68029520312135006 ) ) ;
#3477 = CARTESIAN_POINT ( 'NONE',  ( -16.60513711880302878, 99.50000000000000000, 15.15667007515659570 ) ) ;
#3478 = CARTESIAN_POINT ( 'NONE',  ( 1.653273178848927064E-15, 1.599999997815050312, -27.00000000000000355 ) ) ;
#3479 = ADVANCED_FACE ( 'NONE', ( #774 ), #1341, .T. ) ;
#3480 = LINE ( 'NONE', #240, #8974 ) ;
#3481 = CARTESIAN_POINT ( 'NONE',  ( 21.47055288461538325, 99.50000000000000000, -0.7081330128205128860 ) ) ;
#3482 = EDGE_LOOP ( 'NONE', ( #5224, #3659, #4768, #2811 ) ) ;
#3483 = DIRECTION ( 'NONE',  ( 0.000000000000000000, -1.000000000000000000, 0.000000000000000000 ) ) ;
#3484 = CARTESIAN_POINT ( 'NONE',  ( 27.43301270000000258, 2.749999998907525445, 0.000000000000000000 ) ) ;
#3485 = CARTESIAN_POINT ( 'NONE',  ( -1.250000000000000222, -2.268749998770965615, -2.165063509461096825 ) ) ;
#3486 = CARTESIAN_POINT ( 'NONE',  ( 4.154273145530666511, 99.99999999999997158, -22.82723029927519676 ) ) ;
#3487 = CARTESIAN_POINT ( 'NONE',  ( 7.826802610544922878, 99.99999999999994316, 21.21129867192371421 ) ) ;
#3488 = CARTESIAN_POINT ( 'NONE',  ( 9.881472129446523311, 99.50000000000002842, 20.94326683228310060 ) ) ;
#3489 = CARTESIAN_POINT ( 'NONE',  ( -27.00000000000001421, 3.449999997815051511, 11.18376618407356382 ) ) ;
#3490 = CARTESIAN_POINT ( 'NONE',  ( -21.07003209069497984, 99.49999999999998579, -11.28505157174820361 ) ) ;
#3491 = CARTESIAN_POINT ( 'NONE',  ( -21.52330660073277002, 99.50000000000001421, -9.647028226243550719 ) ) ;
#3492 = CARTESIAN_POINT ( 'NONE',  ( -22.11394672483139701, 99.50000000000000000, -10.91855052283267646 ) ) ;
#3493 = DIRECTION ( 'NONE',  ( 0.000000000000000000, -1.000000000000000000, 0.000000000000000000 ) ) ;
#3494 = DIRECTION ( 'NONE',  ( -0.000000000000000000, 1.000000000000000000, -0.000000000000000000 ) ) ;
#3495 = VERTEX_POINT ( 'NONE', #7941 ) ;
#3496 = EDGE_CURVE ( 'NONE', #1490, #7639, #8571, .T. ) ;
#3497 = CARTESIAN_POINT ( 'NONE',  ( -1.249999999999998224, -0.3749999999999999445, 2.165063509461097713 ) ) ;
#3498 = CARTESIAN_POINT ( 'NONE',  ( -14.89910828679519739, 99.99999999999995737, 16.44921749203638939 ) ) ;
#3499 = CARTESIAN_POINT ( 'NONE',  ( 2.983739933759421259, 99.49999999999998579, -23.28421226151478152 ) ) ;
#3500 = CARTESIAN_POINT ( 'NONE',  ( 27.43301270000000258, 2.649999998907525356, 0.000000000000000000 ) ) ;
#3501 = FACE_OUTER_BOUND ( 'NONE', #8346, .T. ) ;
#3502 = CARTESIAN_POINT ( 'NONE',  ( -20.63200021313574695, 100.0000000000000000, -10.19493994959453431 ) ) ;
#3503 = LINE ( 'NONE', #5909, #7321 ) ;
#3504 = CARTESIAN_POINT ( 'NONE',  ( 0.000000000000000000, 0.000000000000000000, 0.000000000000000000 ) ) ;
#3505 = ORIENTED_EDGE ( 'NONE', *, *, #4960, .F. ) ;
#3506 = CARTESIAN_POINT ( 'NONE',  ( 6.246869686064662197, 99.50000000000000000, 20.92172973853146090 ) ) ;
#3507 = CARTESIAN_POINT ( 'NONE',  ( 3.411785164761435674, 100.0000000000000000, -22.76693382491622231 ) ) ;
#3508 = CARTESIAN_POINT ( 'NONE',  ( 11.36312591709336850, 4.899999998907527576, 27.43301269999999903 ) ) ;
#3509 = CARTESIAN_POINT ( 'NONE',  ( 1.679787559701184688E-15, 0.4499999989075252338, -27.43301270000000258 ) ) ;
#3510 = CARTESIAN_POINT ( 'NONE',  ( 9.877377282685029372E-16, -1.631249998770965659, 2.500000000000000000 ) ) ;
#3511 = CARTESIAN_POINT ( 'NONE',  ( 4.486604876299897349, 99.50000000000000000, -21.85617661337775885 ) ) ;
#3512 = CARTESIAN_POINT ( 'NONE',  ( 4.100286767325537873, 99.50000000000000000, -22.51382885696750336 ) ) ;
#3513 = COLOUR_RGB ( '',0.8941176470588234615, 0.8941176470588234615, 0.8941176470588234615 ) ;
#3514 = DIRECTION ( 'NONE',  ( 0.000000000000000000, -1.000000000000000000, 0.000000000000000000 ) ) ;
#3515 = ORIENTED_EDGE ( 'NONE', *, *, #5959, .T. ) ;
#3516 = ORIENTED_EDGE ( 'NONE', *, *, #4103, .F. ) ;
#3517 = LINE ( 'NONE', #5873, #6712 ) ;
#3518 = CARTESIAN_POINT ( 'NONE',  ( 2.256430356250000102, -1.378124999385482941, -2.763330213280484622E-16 ) ) ;
#3519 = ORIENTED_EDGE ( 'NONE', *, *, #820, .T. ) ;
#3520 = EDGE_CURVE ( 'NONE', #4835, #2411, #2016, .T. ) ;
#3521 = APPLICATION_CONTEXT ( 'automotive_design' ) ;
#3522 = CARTESIAN_POINT ( 'NONE',  ( -22.51488550592518934, 99.99999999999997158, -10.97145172607810615 ) ) ;
#3523 = LINE ( 'NONE', #6708, #1276 ) ;
#3524 = DIRECTION ( 'NONE',  ( -0.000000000000000000, -1.000000000000000000, 0.000000000000000000 ) ) ;
#3525 = VECTOR ( 'NONE', #6198, 1000.000000000000227 ) ;
#3526 = ORIENTED_EDGE ( 'NONE', *, *, #1028, .F. ) ;
#3527 = CARTESIAN_POINT ( 'NONE',  ( -10.49999999999999822, 105.0000000000000142, 0.000000000000000000 ) ) ;
#3528 = CARTESIAN_POINT ( 'NONE',  ( -2.499999999999999112, -3.562500000000000444, 1.443375672974065882 ) ) ;
#3529 = CARTESIAN_POINT ( 'NONE',  ( 0.6698729810778025762, -3.861153809338631504, 2.500000000000002665 ) ) ;
#3530 = CARTESIAN_POINT ( 'NONE',  ( 9.897596448871711416, 99.99999999999998579, 20.85734708541456328 ) ) ;
#3531 = VERTEX_POINT ( 'NONE', #10354 ) ;
#3532 = CARTESIAN_POINT ( 'NONE',  ( 0.000000000000000000, 100.0000000000000000, 0.000000000000000000 ) ) ;
#3533 = CARTESIAN_POINT ( 'NONE',  ( 19.39806930854668110, 2.849999998907525089, -19.39806930854668110 ) ) ;
#3534 = DIRECTION ( 'NONE',  ( -0.000000000000000000, 1.000000000000000000, -0.000000000000000000 ) ) ;
#3535 = CIRCLE ( 'NONE', #6036, 22.50000000000000355 ) ;
#3536 = CARTESIAN_POINT ( 'NONE',  ( 1.034219503716432668E-14, -4.612500000000000711, -2.500000000000000000 ) ) ;
#3537 = CARTESIAN_POINT ( 'NONE',  ( 7.913184448816831029, 99.50000000000000000, 20.09878816755126252 ) ) ;
#3538 = ORIENTED_EDGE ( 'NONE', *, *, #3153, .F. ) ;
#3539 = CARTESIAN_POINT ( 'NONE',  ( 2.852289972453743161, 99.50000000000000000, -22.14293542748032451 ) ) ;
#3540 = CARTESIAN_POINT ( 'NONE',  ( -11.18376618407356560, 4.849999997815050534, -27.00000000000000355 ) ) ;
#3541 = LINE ( 'NONE', #2516, #9546 ) ;
#3542 = FACE_OUTER_BOUND ( 'NONE', #1652, .T. ) ;
#3543 = FACE_OUTER_BOUND ( 'NONE', #6903, .T. ) ;
#3544 = VECTOR ( 'NONE', #4149, 1000.000000000000000 ) ;
#3545 = FACE_OUTER_BOUND ( 'NONE', #1263, .T. ) ;
#3546 = CARTESIAN_POINT ( 'NONE',  ( 2.852289972453743161, 100.0000000000000000, -22.14293542748032451 ) ) ;
#3547 = CARTESIAN_POINT ( 'NONE',  ( -2.499999999999999112, -2.212499999999999467, 1.443375672974065882 ) ) ;
#3548 = ORIENTED_EDGE ( 'NONE', *, *, #3197, .F. ) ;
#3549 = CARTESIAN_POINT ( 'NONE',  ( 5.302876193624534821E-16, -1.687499999999999778, 2.886751345948128655 ) ) ;
#3550 = CONTEXT_DEPENDENT_SHAPE_REPRESENTATION ( #5336, #10104 ) ;
#3551 = CARTESIAN_POINT ( 'NONE',  ( -14.74935495356232984, 100.0000000000000000, 15.91322402822111926 ) ) ;
#3552 = CARTESIAN_POINT ( 'NONE',  ( 5.825495487346713297, 99.50000000000000000, 20.69456627699299744 ) ) ;
#3553 = AXIS2_PLACEMENT_3D ( 'NONE', #6783, #8410, #7513 ) ;
#3554 = CARTESIAN_POINT ( 'NONE',  ( -19.39806930854667755, 3.749999998907525445, -19.39806930854668110 ) ) ;
#3555 = CARTESIAN_POINT ( 'NONE',  ( 2.500000000000000444, -0.6562499987709659033, 1.443375672974063439 ) ) ;
#3556 = CIRCLE ( 'NONE', #1722, 18.00000000000000000 ) ;
#3557 = EDGE_CURVE ( 'NONE', #7033, #1713, #32, .T. ) ;
#3558 = CARTESIAN_POINT ( 'NONE',  ( 4.996790860652426159E-15, -1.856249998770965748, -2.500000000000000000 ) ) ;
#3559 = CARTESIAN_POINT ( 'NONE',  ( 10.72103337977569204, 99.50000000000000000, 22.20268488987243316 ) ) ;
#3560 = CARTESIAN_POINT ( 'NONE',  ( 7.726884419709978857, 100.0000000000000000, 20.74516479202295471 ) ) ;
#3561 = VERTEX_POINT ( 'NONE', #2181 ) ;
#3562 = CARTESIAN_POINT ( 'NONE',  ( 8.393217272293057363, 99.50000000000000000, 19.69436072183531650 ) ) ;
#3563 = CARTESIAN_POINT ( 'NONE',  ( -0.6698729810778020211, -4.142403810567665268, -2.500000000000002665 ) ) ;
#3564 = CARTESIAN_POINT ( 'NONE',  ( -2.256430356250000102, -0.5906249993854828517, 0.000000000000000000 ) ) ;
#3565 =( BOUNDED_SURFACE ( )  B_SPLINE_SURFACE ( 1, 2, ( 
 ( #7816, #3011, #8711, #4724, #3734, #1430, #2894, #3060, #9327, #7705, #751, #2271, #6133, #541, #2321, #5520, #6078, #2159, #644, #3788, #2102, #7918, #3116, #4567, #3943, #8660, #7128, #6188, #1482, #8493, #5469, #9269, #8549, #6973, #1374, #7866, #5296, #10115, #1322, #3891, #4510, #6243, #593, #2952, #7762, #9443, #10175, #4624, #2214, #696, #7078, #3840, #7025, #10228, #6299, #9497, #3166, #4189, #4046, #2421, #5720, #164, #6544, #3261, #7970, #1686, #804, #6451, #7181, #9590, #2528, #4774, #5567, #5766, #8858, #4968, #4879, #8806, #3352, #6351, #8075, #8024, #3310, #9733, #5670, #8757, #1771, #3997, #8905, #13, #4827, #2368, #904, #2571, #7329, #9641, #4094, #7280, #8954, #65, #8166 ),
 ( #6499, #9544, #5618, #3214, #2475, #1581, #1732, #4923, #118, #8120, #6399, #9688, #855, #1635, #996, #950, #7229, #4144, #10333, #2616, #6589, #4391, #5065, #1974, #5963, #7471, #2718, #5906, #8420, #7576, #1821, #3610, #261, #9939, #4239, #2773, #7420, #313, #414, #212, #7522, #1046, #6638, #9992, #8369, #2665, #9833, #9201, #3500, #6742, #363, #1872, #9780, #5221, #8316, #2828, #5118, #3448, #6686, #4287, #7371, #9879, #6793, #1147, #5811, #9156, #9102, #4338, #6009, #5857, #3554, #3397, #5170, #8267, #9053, #1199, #2026, #9002, #1251, #1095, #1923, #5017, #8213, #7687, #2876, #6060, #3827, #2992, #6899, #7009, #3770, #10212, #9427, #3665, #9251, #2084, #10041, #3046, #5342, #4441, #6226 ) ),
 .UNSPECIFIED., .F., .F., .F. ) 
 B_SPLINE_SURFACE_WITH_KNOTS ( ( 2, 2 ),
 ( 3, 2, 2, 2, 2, 2, 2, 2, 2, 2, 2, 2, 2, 2, 2, 2, 2, 2, 2, 2, 2, 2, 2, 2, 2, 2, 2, 2, 2, 2, 2, 2, 2, 2, 2, 2, 2, 2, 2, 2, 2, 2, 2, 2, 2, 2, 2, 2, 2, 2, 3 ),
 ( 0.000000000000000000, 1.000000000000000000 ),
 ( 0.000000000000000000, 0.01785714285714285615, 0.03571428571428571230, 0.05357142857142856845, 0.07142857142857142461, 0.08928571428571428770, 0.1071428571428571369, 0.1250000000000000000, 0.1428571428571428492, 0.1607142857142857262, 0.1785714285714285754, 0.1964285714285714246, 0.2142857142857142738, 0.2321428571428571508, 0.2500000000000000000, 0.2678571428571428492, 0.2857142857142856984, 0.3035714285714285476, 0.3214285714285714524, 0.3392857142857143016, 0.3571428571428571508, 0.3750000000000000000, 0.3928571428571428492, 0.4107142857142856984, 0.4285714285714285476, 0.4464285714285714524, 0.4642857142857143016, 0.4821428571428571508, 0.5000000000000000000, 0.5178571428571429047, 0.5357142857142856984, 0.5535714285714286031, 0.5714285714285713969, 0.5892857142857143016, 0.6071428571428570953, 0.6250000000000000000, 0.6428571428571429047, 0.6607142857142856984, 0.6785714285714286031, 0.6964285714285713969, 0.7142857142857143016, 0.7321428571428570953, 0.7500000000000000000, 0.7678571428571429047, 0.7857142857142856984, 0.8035714285714286031, 0.8214285714285713969, 0.8392857142857143016, 0.8571428571428570953, 0.8750000000000000000, 0.8928571428571429047 ),
 .UNSPECIFIED. ) 
 GEOMETRIC_REPRESENTATION_ITEM ( )  RATIONAL_B_SPLINE_SURFACE ( (
 ( 1.000000000000000000, 0.9238795325112867385, 1.000000000000000000, 0.9238795325112867385, 1.000000000000000000, 0.9238795325112867385, 1.000000000000000000, 0.9238795325112867385, 1.000000000000000000, 0.9238795325112867385, 1.000000000000000000, 0.9238795325112867385, 1.000000000000000000, 0.9238795325112867385, 1.000000000000000000, 0.9238795325112867385, 1.000000000000000000, 0.9238795325112867385, 1.000000000000000000, 0.9238795325112867385, 1.000000000000000000, 0.9238795325112867385, 1.000000000000000000, 0.9238795325112867385, 1.000000000000000000, 0.9238795325112867385, 1.000000000000000000, 0.9238795325112867385, 1.000000000000000000, 0.9238795325112867385, 1.000000000000000000, 0.9238795325112867385, 1.000000000000000000, 0.9238795325112867385, 1.000000000000000000, 0.9238795325112867385, 1.000000000000000000, 0.9238795325112867385, 1.000000000000000000, 0.9238795325112867385, 1.000000000000000000, 0.9238795325112867385, 1.000000000000000000, 0.9238795325112867385, 1.000000000000000000, 0.9238795325112867385, 1.000000000000000000, 0.9238795325112867385, 1.000000000000000000, 0.9238795325112867385, 1.000000000000000000, 0.9238795325112867385, 1.000000000000000000, 0.9238795325112867385, 1.000000000000000000, 0.9238795325112867385, 1.000000000000000000, 0.9238795325112867385, 1.000000000000000000, 0.9238795325112867385, 1.000000000000000000, 0.9238795325112867385, 1.000000000000000000, 0.9238795325112867385, 1.000000000000000000, 0.9238795325112867385, 1.000000000000000000, 0.9238795325112867385, 1.000000000000000000, 0.9238795325112867385, 1.000000000000000000, 0.9238795325112867385, 1.000000000000000000, 0.9238795325112867385, 1.000000000000000000, 0.9238795325112867385, 1.000000000000000000, 0.9238795325112867385, 1.000000000000000000, 0.9238795325112867385, 1.000000000000000000, 0.9238795325112867385, 1.000000000000000000, 0.9238795325112867385, 1.000000000000000000, 0.9238795325112867385, 1.000000000000000000, 0.9238795325112867385, 1.000000000000000000, 0.9238795325112867385, 1.000000000000000000, 0.9238795325112867385, 1.000000000000000000, 0.9238795325112867385, 1.000000000000000000, 0.9238795325112867385, 1.000000000000000000, 0.9238795325112867385, 1.000000000000000000, 0.9238795325112867385, 1.000000000000000000),
 ( 1.000000000000000000, 0.9238795325112867385, 1.000000000000000000, 0.9238795325112867385, 1.000000000000000000, 0.9238795325112867385, 1.000000000000000000, 0.9238795325112867385, 1.000000000000000000, 0.9238795325112867385, 1.000000000000000000, 0.9238795325112867385, 1.000000000000000000, 0.9238795325112867385, 1.000000000000000000, 0.9238795325112867385, 1.000000000000000000, 0.9238795325112867385, 1.000000000000000000, 0.9238795325112867385, 1.000000000000000000, 0.9238795325112867385, 1.000000000000000000, 0.9238795325112867385, 1.000000000000000000, 0.9238795325112867385, 1.000000000000000000, 0.9238795325112867385, 1.000000000000000000, 0.9238795325112867385, 1.000000000000000000, 0.9238795325112867385, 1.000000000000000000, 0.9238795325112867385, 1.000000000000000000, 0.9238795325112867385, 1.000000000000000000, 0.9238795325112867385, 1.000000000000000000, 0.9238795325112867385, 1.000000000000000000, 0.9238795325112867385, 1.000000000000000000, 0.9238795325112867385, 1.000000000000000000, 0.9238795325112867385, 1.000000000000000000, 0.9238795325112867385, 1.000000000000000000, 0.9238795325112867385, 1.000000000000000000, 0.9238795325112867385, 1.000000000000000000, 0.9238795325112867385, 1.000000000000000000, 0.9238795325112867385, 1.000000000000000000, 0.9238795325112867385, 1.000000000000000000, 0.9238795325112867385, 1.000000000000000000, 0.9238795325112867385, 1.000000000000000000, 0.9238795325112867385, 1.000000000000000000, 0.9238795325112867385, 1.000000000000000000, 0.9238795325112867385, 1.000000000000000000, 0.9238795325112867385, 1.000000000000000000, 0.9238795325112867385, 1.000000000000000000, 0.9238795325112867385, 1.000000000000000000, 0.9238795325112867385, 1.000000000000000000, 0.9238795325112867385, 1.000000000000000000, 0.9238795325112867385, 1.000000000000000000, 0.9238795325112867385, 1.000000000000000000, 0.9238795325112867385, 1.000000000000000000, 0.9238795325112867385, 1.000000000000000000, 0.9238795325112867385, 1.000000000000000000, 0.9238795325112867385, 1.000000000000000000, 0.9238795325112867385, 1.000000000000000000, 0.9238795325112867385, 1.000000000000000000, 0.9238795325112867385, 1.000000000000000000, 0.9238795325112867385, 1.000000000000000000, 0.9238795325112867385, 1.000000000000000000) ) ) 
 REPRESENTATION_ITEM ( '' )  SURFACE ( )  );
#3566 = CARTESIAN_POINT ( 'NONE',  ( 9.563602730896748838, 99.50000000000001421, 20.87184380654744587 ) ) ;
#3567 = CARTESIAN_POINT ( 'NONE',  ( 3.845216150098881513, 100.0000000000000000, -21.40922359334548020 ) ) ;
#3568 = DIRECTION ( 'NONE',  ( 0.000000000000000000, 0.000000000000000000, -1.000000000000000000 ) ) ;
#3569 = CARTESIAN_POINT ( 'NONE',  ( 11.18376618407357093, 2.550000000000000266, -27.00000000000000355 ) ) ;
#3570 = EDGE_LOOP ( 'NONE', ( #1013, #416 ) ) ;
#3571 = EDGE_CURVE ( 'NONE', #9254, #3171, #10280, .T. ) ;
#3572 = ORIENTED_EDGE ( 'NONE', *, *, #10251, .T. ) ;
#3573 = CARTESIAN_POINT ( 'NONE',  ( 4.906732565843439531, 100.0000000000000142, -23.57187248890526376 ) ) ;
#3574 = CARTESIAN_POINT ( 'NONE',  ( 1.128215178124999607, -1.303124999385482985, -1.954126010382871259 ) ) ;
#3575 = ORIENTED_EDGE ( 'NONE', *, *, #6979, .F. ) ;
#3576 = CARTESIAN_POINT ( 'NONE',  ( -22.00707282958688182, 99.49999999999997158, -9.748971510896797810 ) ) ;
#3577 = DIRECTION ( 'NONE',  ( -0.9985315370676781654, 0.000000000000000000, 0.05417351272771728926 ) ) ;
#3578 = LINE ( 'NONE', #2741, #6260 ) ;
#3579 = CARTESIAN_POINT ( 'NONE',  ( 4.331079892889020400, 100.0000000000000284, -24.67336562508343079 ) ) ;
#3580 = ADVANCED_FACE ( 'NONE', ( #5380 ), #1397, .F. ) ;
#3581 = EDGE_CURVE ( 'NONE', #471, #2983, #610, .T. ) ;
#3582 = VECTOR ( 'NONE', #6132, 1000.000000000000000 ) ;
#3583 = CARTESIAN_POINT ( 'NONE',  ( -15.13520964245927836, 99.49999999999998579, 15.69931698147095034 ) ) ;
#3584 = CYLINDRICAL_SURFACE ( 'NONE', #4979, 2.500000000000000000 ) ;
#3585 = ORIENTED_EDGE ( 'NONE', *, *, #3638, .T. ) ;
#3586 = CARTESIAN_POINT ( 'NONE',  ( 9.184850993605147944E-16, 85.00000000000000000, 7.500000000000000000 ) ) ;
#3587 = CARTESIAN_POINT ( 'NONE',  ( 1.250000000000001110, -2.549999999999999822, 2.165063509461096380 ) ) ;
#3588 = ORIENTED_EDGE ( 'NONE', *, *, #4727, .T. ) ;
#3589 = PLANE ( 'NONE',  #6901 ) ;
#3590 = CARTESIAN_POINT ( 'NONE',  ( 11.36312591709336139, 3.699999998907525622, -27.43301270000000258 ) ) ;
#3591 = DIRECTION ( 'NONE',  ( 0.000000000000000000, -1.000000000000000000, 0.000000000000000000 ) ) ;
#3592 = CARTESIAN_POINT ( 'NONE',  ( -16.85368146453285831, 99.99999999999998579, 16.27421966797335529 ) ) ;
#3593 = CARTESIAN_POINT ( 'NONE',  ( -4.959819536546781389E-15, 4.399999997815050357, 27.00000000000000355 ) ) ;
#3594 = AXIS2_PLACEMENT_3D ( 'NONE', #247, #2812, #5797 ) ;
#3595 = ORIENTED_EDGE ( 'NONE', *, *, #1064, .T. ) ;
#3596 = CARTESIAN_POINT ( 'NONE',  ( -19.46743691185369585, 99.50000000000000000, -8.912588186774021537 ) ) ;
#3597 = CARTESIAN_POINT ( 'NONE',  ( -19.09188309203678457, 4.099999997815050534, -19.09188309203678813 ) ) ;
#3598 = CARTESIAN_POINT ( 'NONE',  ( 24.91446314102564230, 99.50000000000000000, -1.581029647435897578 ) ) ;
#3599 = PLANE ( 'NONE',  #10350 ) ;
#3600 = CARTESIAN_POINT ( 'NONE',  ( 3.000000000000000000, -15.00000000000000000, -1.732050807568876749 ) ) ;
#3601 = VERTEX_POINT ( 'NONE', #8628 ) ;
#3602 = CARTESIAN_POINT ( 'NONE',  ( 4.829054701479813083, 99.50000000000000000, -23.91032069601275367 ) ) ;
#3603 = CARTESIAN_POINT ( 'NONE',  ( 19.39806930854667399, 1.849999998907525312, 19.39806930854668465 ) ) ;
#3604 = EDGE_LOOP ( 'NONE', ( #2194, #4615, #9752, #6085 ) ) ;
#3605 = CARTESIAN_POINT ( 'NONE',  ( 1.250000000000001110, -1.199999999999999956, 2.165063509461096380 ) ) ;
#3606 =( NAMED_UNIT ( * ) SI_UNIT ( $, .STERADIAN. ) SOLID_ANGLE_UNIT ( ) );
#3607 = CARTESIAN_POINT ( 'NONE',  ( 0.000000000000000000, 0.000000000000000000, 0.000000000000000000 ) ) ;
#3608 = AXIS2_PLACEMENT_3D ( 'NONE', #1375, #4568, #1531 ) ;
#3609 = CARTESIAN_POINT ( 'NONE',  ( -1.128215178124998497, -0.6281249993854828295, 1.954126010382872147 ) ) ;
#3610 = CARTESIAN_POINT ( 'NONE',  ( 27.43301269999999548, 1.799999998907525267, 11.36312591709337738 ) ) ;
#3611 = DIRECTION ( 'NONE',  ( -0.000000000000000000, 1.000000000000000000, -0.000000000000000000 ) ) ;
#3613 = VERTEX_POINT ( 'NONE', #9407 ) ;
#3612 = VERTEX_POINT ( 'NONE', #6994 ) ;
#3614 = CARTESIAN_POINT ( 'NONE',  ( -15.62070810370258833, 100.0000000000000000, 16.62245103965875970 ) ) ;
#3615 = CARTESIAN_POINT ( 'NONE',  ( 4.523042264738025509, 100.0000000000000142, -24.25177047807976294 ) ) ;
#3616 =( NAMED_UNIT ( * ) PLANE_ANGLE_UNIT ( ) SI_UNIT ( $, .RADIAN. ) );
#3617 = CARTESIAN_POINT ( 'NONE',  ( -18.01369080470046313, 99.50000000000000000, 17.15556831233607937 ) ) ;
#3618 = AXIS2_PLACEMENT_3D ( 'NONE', #3964, #9514, #3327 ) ;
#3619 = CARTESIAN_POINT ( 'NONE',  ( 3.061616997868383141E-16, -5.000000000000000000, 2.500000000000000000 ) ) ;
#3620 = CARTESIAN_POINT ( 'NONE',  ( 4.793167276645844410, 99.99999999999998579, -21.69837440717521204 ) ) ;
#3621 = VERTEX_POINT ( 'NONE', #2236 ) ;
#3622 = EDGE_CURVE ( 'NONE', #8050, #1968, #4643, .T. ) ;
#3623 = CARTESIAN_POINT ( 'NONE',  ( -1.595409442497313560E-16, -0.2531249993854829405, -2.605501347177161087 ) ) ;
#3624 = CARTESIAN_POINT ( 'NONE',  ( 27.43301270000000258, 1.049999998907525267, 0.000000000000000000 ) ) ;
#3625 = EDGE_CURVE ( 'NONE', #7937, #5423, #6931, .T. ) ;
#3626 = CARTESIAN_POINT ( 'NONE',  ( 27.00000000000000355, 4.850000000000000533, -11.18376618407356915 ) ) ;
#3627 = CARTESIAN_POINT ( 'NONE',  ( 3.477525819554967423, 99.50000000000000000, -22.44236894434852658 ) ) ;
#3628 = VECTOR ( 'NONE', #9569, 1000.000000000000000 ) ;
#3629 = PLANE ( 'NONE',  #9470 ) ;
#3630 = CARTESIAN_POINT ( 'NONE',  ( 0.000000000000000000, -25.00000000000000000, 0.000000000000000000 ) ) ;
#3631 = AXIS2_PLACEMENT_3D ( 'NONE', #2767, #4233, #5110 ) ;
#3632 = CARTESIAN_POINT ( 'NONE',  ( 2.256430356250000546, -0.9656249993854827407, 1.302750673588579877 ) ) ;
#3633 = ORIENTED_EDGE ( 'NONE', *, *, #3915, .T. ) ;
#3634 = CARTESIAN_POINT ( 'NONE',  ( 0.000000000000000000, 100.0000000000000000, 0.000000000000000000 ) ) ;
#3635 = CARTESIAN_POINT ( 'NONE',  ( -16.07368679829020763, 100.0000000000000000, 17.11560437002838952 ) ) ;
#3636 =( GEOMETRIC_REPRESENTATION_CONTEXT ( 3 ) GLOBAL_UNCERTAINTY_ASSIGNED_CONTEXT ( ( #6959 ) ) GLOBAL_UNIT_ASSIGNED_CONTEXT ( ( #9686, #1867, #3445 ) ) REPRESENTATION_CONTEXT ( 'NONE', 'WORKASPACE' ) );
#3637 = EDGE_CURVE ( 'NONE', #1777, #3208, #1178, .T. ) ;
#3638 = EDGE_CURVE ( 'NONE', #3821, #2104, #9171, .T. ) ;
#3639 = CARTESIAN_POINT ( 'NONE',  ( 4.100286767325537873, 100.0000000000000000, -22.51382885696750336 ) ) ;
#3640 = CARTESIAN_POINT ( 'NONE',  ( -19.09188309203678457, 3.299999997815050712, -19.09188309203678813 ) ) ;
#3641 = CARTESIAN_POINT ( 'NONE',  ( 1.250000000000001110, -0.6937499987709658811, 2.165063509461096380 ) ) ;
#3642 = CARTESIAN_POINT ( 'NONE',  ( -27.00000000000000355, 1.200000000000000178, -3.306546357697854128E-15 ) ) ;
#3643 = CARTESIAN_POINT ( 'NONE',  ( 0.6698729810778112359, -2.832596189432333933, -2.499999999999996447 ) ) ;
#3644 = VERTEX_POINT ( 'NONE', #8777 ) ;
#3645 = PLANE ( 'NONE',  #10262 ) ;
#3646 = CARTESIAN_POINT ( 'NONE',  ( 27.43301270000000258, 3.599999998907525534, -11.36312591709336139 ) ) ;
#3647 = CARTESIAN_POINT ( 'NONE',  ( 9.676361905416719367, 99.50000000000000000, 21.63547735782115211 ) ) ;
#3648 = CIRCLE ( 'NONE', #7997, 17.50000000000000355 ) ;
#3649 = CARTESIAN_POINT ( 'NONE',  ( -16.35834224700816009, 99.50000000000000000, 16.43761959438736397 ) ) ;
#3650 = VERTEX_POINT ( 'NONE', #6564 ) ;
#3651 = CARTESIAN_POINT ( 'NONE',  ( -0.6698729810778054627, -0.7513461882033000139, 2.500000000000000000 ) ) ;
#3652 = CARTESIAN_POINT ( 'NONE',  ( 9.357053078540884528, 99.50000000000001421, 19.70216357796830664 ) ) ;
#3653 = DIRECTION ( 'NONE',  ( 0.000000000000000000, 0.000000000000000000, -1.000000000000000000 ) ) ;
#3654 = CARTESIAN_POINT ( 'NONE',  ( 0.000000000000000000, 75.00000000000001421, 0.000000000000000000 ) ) ;
#3655 = CARTESIAN_POINT ( 'NONE',  ( -21.94169572595625795, 100.0000000000000000, -9.715372641902229489 ) ) ;
#3656 = VERTEX_POINT ( 'NONE', #1702 ) ;
#3657 = CARTESIAN_POINT ( 'NONE',  ( -15.32348647777738826, 99.50000000000000000, 15.39505148541300450 ) ) ;
#3658 = CARTESIAN_POINT ( 'NONE',  ( 19.39806930854667399, 1.049999998907525045, 19.39806930854668465 ) ) ;
#3659 = ORIENTED_EDGE ( 'NONE', *, *, #2238, .F. ) ;
#3660 = ADVANCED_FACE ( 'NONE', ( #6472 ), #4066, .T. ) ;
#3661 = CARTESIAN_POINT ( 'NONE',  ( -1.767625397874844694E-16, -0.5625000000000000000, -2.886751345948128655 ) ) ;
#3662 = DIRECTION ( 'NONE',  ( 0.000000000000000000, 0.000000000000000000, 1.000000000000000000 ) ) ;
#3663 = CARTESIAN_POINT ( 'NONE',  ( 3.638175769014108774, 99.99999999999995737, -21.10017783766535970 ) ) ;
#3664 = CARTESIAN_POINT ( 'NONE',  ( -2.256430356250000102, -1.603124999385482807, 0.000000000000000000 ) ) ;
#3665 = CARTESIAN_POINT ( 'NONE',  ( 11.36312591709336850, 4.899999998907526688, 27.43301269999999903 ) ) ;
#3666 = CARTESIAN_POINT ( 'NONE',  ( -11.36312591709335962, 2.999999998907524557, -27.43301270000000258 ) ) ;
#3667 = ORIENTED_EDGE ( 'NONE', *, *, #6650, .T. ) ;
#3668 = B_SPLINE_CURVE_WITH_KNOTS ( 'NONE', 3,
 ( #9687, #1529, #5616, #4723, #4826, #2526, #750, #5718, #1730, #9049, #4187, #8313, #4336, #5063, #1145 ),
 .UNSPECIFIED., .F., .F.,
 ( 4, 1, 1, 1, 1, 1, 1, 1, 1, 1, 1, 1, 4 ),
 ( 0.000000000000000000, 0.08635447908391848115, 0.1695936995346988552, 0.2509241109261274860, 0.3325843554298174576, 0.4138183564518133073, 0.4948404748415979881, 0.5772065644957810049, 0.6619893985813737336, 0.7474108716807353892, 0.8313115314839791825, 0.9147691218156368542, 1.000000000000000000 ),
 .UNSPECIFIED. ) ;
#3669 = CARTESIAN_POINT ( 'NONE',  ( -15.42956291708403782, 99.99999999999998579, 16.53061251458192515 ) ) ;
#3670 = CARTESIAN_POINT ( 'NONE',  ( 8.132491713109025966, 99.50000000000000000, 21.08089001807756091 ) ) ;
#3671 = CYLINDRICAL_SURFACE ( 'NONE', #2891, 2.500000000000000000 ) ;
#3672 = CARTESIAN_POINT ( 'NONE',  ( -4.959819536546781389E-15, 4.599999999999999645, 27.00000000000000355 ) ) ;
#3673 = CARTESIAN_POINT ( 'NONE',  ( 4.786228327491940187E-16, -1.378124999385482941, 2.605501347177161087 ) ) ;
#3674 = CARTESIAN_POINT ( 'NONE',  ( 3.373335371007685435, 100.0000000000000000, -22.75111425220066863 ) ) ;
#3675 = PLANE ( 'NONE',  #9643 ) ;
#3676 = CARTESIAN_POINT ( 'NONE',  ( 19.39806930854667399, 2.549999998907525267, 19.39806930854668465 ) ) ;
#3677 = CARTESIAN_POINT ( 'NONE',  ( -15.42740294075255925, 99.99999999999995737, 14.91894146668702348 ) ) ;
#3678 = CARTESIAN_POINT ( 'NONE',  ( 9.563602730896748838, 99.50000000000001421, 20.87184380654744587 ) ) ;
#3679 = FACE_OUTER_BOUND ( 'NONE', #5231, .T. ) ;
#3680 = EDGE_LOOP ( 'NONE', ( #9796, #7586, #241, #5335, #3732, #5188, #9994 ) ) ;
#3681 = EDGE_CURVE ( 'NONE', #2280, #653, #3233, .T. ) ;
#3682 = CARTESIAN_POINT ( 'NONE',  ( 0.000000000000000000, -15.00000000000000000, -3.464101615137755275 ) ) ;
#3683 = CARTESIAN_POINT ( 'NONE',  ( -2.256430356249999214, -2.465624999385482852, 1.302750673588581876 ) ) ;
#3684 = ORIENTED_EDGE ( 'NONE', *, *, #5244, .T. ) ;
#3685 = DIRECTION ( 'NONE',  ( 0.000000000000000000, 0.9848077530122080203, -0.1736481776669307198 ) ) ;
#3686 = CARTESIAN_POINT ( 'NONE',  ( -15.24337324910153946, 99.99999999999997158, 16.81353386054630761 ) ) ;
#3687 = CARTESIAN_POINT ( 'NONE',  ( -21.18972881998075763, 99.49999999999998579, -9.781869222470191971 ) ) ;
#3688 = PRESENTATION_LAYER_ASSIGNMENT (  '', '', ( #510 ) ) ;
#3689 = CARTESIAN_POINT ( 'NONE',  ( 3.817429849879703241, 99.49999999999998579, -22.92346308580664171 ) ) ;
#3690 = CARTESIAN_POINT ( 'NONE',  ( -11.18376618407358336, 3.750000000000000444, 26.99999999999999645 ) ) ;
#3691 = B_SPLINE_CURVE_WITH_KNOTS ( 'NONE', 3,
 ( #8749, #8944, #8850, #4916, #1676, #8798, #845, #5710, #1573, #6387, #4818, #1625, #8113, #1762, #988, #7218, #4084, #1724, #9580 ),
 .UNSPECIFIED., .F., .F.,
 ( 4, 1, 1, 1, 1, 1, 1, 1, 1, 1, 1, 1, 1, 1, 1, 1, 4 ),
 ( 0.000000000000000000, 0.05935611633690887623, 0.1167563879513689451, 0.1743885027374874330, 0.2308223543163396840, 0.2888100779544915953, 0.3475404098195560842, 0.4086537266250744316, 0.4723446836969566465, 0.5362968130936018873, 0.6000923674009760456, 0.6637702377379335328, 0.7274568328636339398, 0.7924602533659969028, 0.8590386936388050287, 0.9283644560612371865, 1.000000000000000000 ),
 .UNSPECIFIED. ) ;
#3692 = EDGE_LOOP ( 'NONE', ( #5573, #207, #7888, #9692 ) ) ;
#3693 = EDGE_CURVE ( 'NONE', #7819, #4830, #2593, .T. ) ;
#3694 = FACE_OUTER_BOUND ( 'NONE', #112, .T. ) ;
#3695 = CARTESIAN_POINT ( 'NONE',  ( -1.249999999999998224, -2.568749998770965437, 2.165063509461097713 ) ) ;
#3696 = CARTESIAN_POINT ( 'NONE',  ( 26.99999999999999645, 0.7499999999999998890, 11.18376618407358691 ) ) ;
#3697 = ORIENTED_EDGE ( 'NONE', *, *, #5586, .T. ) ;
#3698 = DIRECTION ( 'NONE',  ( 0.000000000000000000, 0.000000000000000000, -1.000000000000000000 ) ) ;
#3699 = CARTESIAN_POINT ( 'NONE',  ( 11.36312591709336139, 2.899999998907526244, -27.43301270000000258 ) ) ;
#3700 = CARTESIAN_POINT ( 'NONE',  ( 2.256430356250000102, -0.8156249993854829405, -2.763330213280484622E-16 ) ) ;
#3701 = CARTESIAN_POINT ( 'NONE',  ( 9.902568905804752575, 99.99999999999997158, 20.48863403721516363 ) ) ;
#3702 = LINE ( 'NONE', #2919, #6595 ) ;
#3703 = LINE ( 'NONE', #565, #2213 ) ;
#3704 = SURFACE_STYLE_USAGE ( .BOTH. , #7564 ) ;
#3705 = DIRECTION ( 'NONE',  ( 0.000000000000000000, -0.000000000000000000, -1.000000000000000000 ) ) ;
#3706 = EDGE_LOOP ( 'NONE', ( #217, #9083, #327, #10236 ) ) ;
#3707 = DIRECTION ( 'NONE',  ( 0.9197781680807419757, 0.000000000000000000, -0.3924386850477849520 ) ) ;
#3708 = CARTESIAN_POINT ( 'NONE',  ( -5.039362679103552881E-15, 1.749999998907525223, 27.43301270000000258 ) ) ;
#3709 = CIRCLE ( 'NONE', #9402, 1.324999999999999734 ) ;
#3710 = ORIENTED_EDGE ( 'NONE', *, *, #1823, .F. ) ;
#3711 = CARTESIAN_POINT ( 'NONE',  ( -2.499999999999999556, -2.662499999999999645, 1.443375672974065882 ) ) ;
#3712 = APPLICATION_PROTOCOL_DEFINITION ( 'draft international standard', 'automotive_design', 1998, #3146 ) ;
#3713 = CARTESIAN_POINT ( 'NONE',  ( 1.249999999999999334, -2.343749998770965792, -2.165063509461096825 ) ) ;
#3714 = CARTESIAN_POINT ( 'NONE',  ( 3.106448761625311139, 99.99999999999995737, -21.38062202216113761 ) ) ;
#3715 = CARTESIAN_POINT ( 'NONE',  ( -2.256430356250000102, -1.640624999385482896, -1.302750673588580321 ) ) ;
#3716 = EDGE_CURVE ( 'NONE', #7134, #3111, #88, .T. ) ;
#3717 = CARTESIAN_POINT ( 'NONE',  ( -16.92301558088953328, 99.50000000000001421, 15.88693424423437683 ) ) ;
#3718 = CARTESIAN_POINT ( 'NONE',  ( -19.39806930854668465, 0.8499999989075252005, 19.39806930854667755 ) ) ;
#3719 = ORIENTED_EDGE ( 'NONE', *, *, #4168, .F. ) ;
#3720 = UNCERTAINTY_MEASURE_WITH_UNIT (LENGTH_MEASURE( 1.000000000000000082E-05 ), #9441, 'distance_accuracy_value', 'NONE');
#3721 = EDGE_CURVE ( 'NONE', #3778, #8324, #5691, .T. ) ;
#3722 = CARTESIAN_POINT ( 'NONE',  ( -16.34021191015031249, 100.0000000000000000, 16.45483272884350967 ) ) ;
#3723 = FACE_OUTER_BOUND ( 'NONE', #5826, .T. ) ;
#3724 = FACE_OUTER_BOUND ( 'NONE', #9122, .T. ) ;
#3725 = DIRECTION ( 'NONE',  ( 0.1714283378204774499, 0.000000000000000000, -0.9851965920526259968 ) ) ;
#3726 = EDGE_LOOP ( 'NONE', ( #9226, #8690, #6107, #1682 ) ) ;
#3727 = CARTESIAN_POINT ( 'NONE',  ( -2.256430356249998770, -1.903124999385482852, 1.302750673588581876 ) ) ;
#3728 = CARTESIAN_POINT ( 'NONE',  ( -8.673617379884035472E-16, -15.00000000000000000, 3.464101615137756163 ) ) ;
#3729 = VERTEX_POINT ( 'NONE', #9708 ) ;
#3730 = PLANE ( 'NONE',  #5585 ) ;
#3731 = CARTESIAN_POINT ( 'NONE',  ( 1.679787559701184688E-15, 1.249999998907525223, -27.43301270000000258 ) ) ;
#3732 = ORIENTED_EDGE ( 'NONE', *, *, #7105, .F. ) ;
#3733 = DIRECTION ( 'NONE',  ( 0.000000000000000000, 0.000000000000000000, 1.000000000000000000 ) ) ;
#3734 = CARTESIAN_POINT ( 'NONE',  ( 1.653273178848927064E-15, 0.2000000000000000111, -27.00000000000000355 ) ) ;
#3735 = CARTESIAN_POINT ( 'NONE',  ( 8.684839681857363658, 100.0000000000000426, 19.94043386883836178 ) ) ;
#3736 = ORIENTED_EDGE ( 'NONE', *, *, #1402, .T. ) ;
#3737 = FACE_OUTER_BOUND ( 'NONE', #8066, .T. ) ;
#3738 = AXIS2_PLACEMENT_3D ( 'NONE', #5791, #8888, #1025 ) ;
#3739 = CARTESIAN_POINT ( 'NONE',  ( -2.256430356250000102, -1.153124999385482852, 0.000000000000000000 ) ) ;
#3740 = ORIENTED_EDGE ( 'NONE', *, *, #6262, .T. ) ;
#3741 = LINE ( 'NONE', #6923, #8462 ) ;
#3742 = CARTESIAN_POINT ( 'NONE',  ( 19.39806930854668110, 0.3499999989075252560, -19.39806930854668110 ) ) ;
#3743 = CARTESIAN_POINT ( 'NONE',  ( -21.52330660073277002, 99.50000000000001421, -9.647028226243550719 ) ) ;
#3744 = CARTESIAN_POINT ( 'NONE',  ( 2.256430356250000102, -1.378124999385482941, -2.763330213280484622E-16 ) ) ;
#3745 = CARTESIAN_POINT ( 'NONE',  ( 2.983739933759421259, 99.99999999999998579, -23.28421226151478152 ) ) ;
#3746 = CARTESIAN_POINT ( 'NONE',  ( 4.633286773149219329, 99.50000000000002842, -21.44575434969419447 ) ) ;
#3747 = CARTESIAN_POINT ( 'NONE',  ( -16.76168403648438243, 100.0000000000000284, 16.44483764528499847 ) ) ;
#3748 = CARTESIAN_POINT ( 'NONE',  ( 9.877377282685029372E-16, -0.3374999999999999667, 2.500000000000000000 ) ) ;
#3749 = EDGE_LOOP ( 'NONE', ( #2945, #3976, #5575, #7415 ) ) ;
#3750 = DIRECTION ( 'NONE',  ( 0.05468478504300072762, 0.000000000000000000, 0.9985036676371302766 ) ) ;
#3751 = CARTESIAN_POINT ( 'NONE',  ( 2.500000000000000000, -4.274999999999999467, -3.061616997868383141E-16 ) ) ;
#3752 = CARTESIAN_POINT ( 'NONE',  ( -1.128215178125000273, -0.6656249993854830294, -1.954126010382871259 ) ) ;
#3753 = EDGE_CURVE ( 'NONE', #10122, #1438, #2796, .T. ) ;
#3754 = CARTESIAN_POINT ( 'NONE',  ( 9.766630880609509902, 99.50000000000002842, 21.37293705761699059 ) ) ;
#3755 = B_SPLINE_SURFACE_WITH_KNOTS ( 'NONE', 3, 1, ( 
 ( #5930, #3476 ),
 ( #9856, #3579 ),
 ( #6819, #6662 ),
 ( #438, #2594 ),
 ( #9128, #1946 ),
 ( #8978, #1797 ),
 ( #7394, #2228 ),
 ( #5250, #5482 ),
 ( #4691, #8562 ),
 ( #10241, #2849 ),
 ( #7715, #3025 ),
 ( #9457, #2906 ),
 ( #5430, #497 ),
 ( #2056, #1387 ),
 ( #7039, #6146 ),
 ( #1495, #4522 ),
 ( #6201, #2113 ),
 ( #8505, #2283 ),
 ( #6033, #9399 ) ),
 .UNSPECIFIED., .F., .F., .F.,
 ( 4, 1, 1, 1, 1, 1, 1, 1, 1, 1, 1, 1, 1, 1, 1, 1, 4 ),
 ( 2, 2 ),
 ( 0.000000000000000000, 0.06533929434940796699, 0.1284421010879715219, 0.1894557237235162950, 0.2487158350925330053, 0.3070727012892665031, 0.3650088636856013702, 0.4229902474982629723, 0.4815891416229265420, 0.5404453987529589387, 0.6002338948610608238, 0.6608164219703346332, 0.7232441343194829786, 0.7881366429682739039, 0.8556965829275263724, 0.9259544997225339635, 1.000000000000000000 ),
 ( 0.000000000000000000, 1.000000000000000000 ),
 .UNSPECIFIED. ) ;
#3756 = VERTEX_POINT ( 'NONE', #386 ) ;
#3757 = CARTESIAN_POINT ( 'NONE',  ( -22.08823018108446234, 100.0000000000000000, -9.406177930363766038 ) ) ;
#3758 = CARTESIAN_POINT ( 'NONE',  ( 8.429066232339796017, 99.50000000000000000, 19.67794530653910101 ) ) ;
#3759 = CARTESIAN_POINT ( 'NONE',  ( 0.000000000000000000, -5.000000000000000000, 0.000000000000000000 ) ) ;
#3760 = DIRECTION ( 'NONE',  ( 0.000000000000000000, 1.000000000000000000, 0.000000000000000000 ) ) ;
#3761 = VERTEX_POINT ( 'NONE', #8286 ) ;
#3762 = PLANE ( 'NONE',  #2117 ) ;
#3763 = DIRECTION ( 'NONE',  ( 0.000000000000000000, -1.000000000000000000, 0.000000000000000000 ) ) ;
#3764 = VERTEX_POINT ( 'NONE', #8393 ) ;
#3765 = CARTESIAN_POINT ( 'NONE',  ( -1.250000000000000222, -2.774999999999999467, -2.165063509461096825 ) ) ;
#3766 = APPLICATION_PROTOCOL_DEFINITION ( 'draft international standard', 'automotive_design', 1998, #865 ) ;
#3767 = CARTESIAN_POINT ( 'NONE',  ( 27.21650635000000307, 0.4749999983612877563, 0.000000000000000000 ) ) ;
#3768 = CARTESIAN_POINT ( 'NONE',  ( 2.843562173796539749, 99.50000000000001421, -21.91597968833000110 ) ) ;
#3769 = CARTESIAN_POINT ( 'NONE',  ( -2.256430356250000102, -2.990624999385482763, -1.302750673588580321 ) ) ;
#3770 = CARTESIAN_POINT ( 'NONE',  ( -19.39806930854668465, 4.749999998907525445, 19.39806930854667755 ) ) ;
#3771 = CARTESIAN_POINT ( 'NONE',  ( 1.679787559701184688E-15, 1.349999998907525312, -27.43301270000000258 ) ) ;
#3772 = VERTEX_POINT ( 'NONE', #5983 ) ;
#3773 = CARTESIAN_POINT ( 'NONE',  ( -15.49014769301379069, 99.99999999999997158, 16.56834637662448273 ) ) ;
#3774 = FACE_OUTER_BOUND ( 'NONE', #5033, .T. ) ;
#3775 = FACE_OUTER_BOUND ( 'NONE', #9335, .T. ) ;
#3776 = VECTOR ( 'NONE', #9104, 999.9999999999998863 ) ;
#3777 = CARTESIAN_POINT ( 'NONE',  ( -16.05932294508833280, 100.0000000000000000, 15.21084698918278555 ) ) ;
#3778 = VERTEX_POINT ( 'NONE', #2691 ) ;
#3779 = CARTESIAN_POINT ( 'NONE',  ( 2.256430356249999658, -0.3281249993854829516, -1.302750673588581432 ) ) ;
#3780 = CARTESIAN_POINT ( 'NONE',  ( 4.280752963211088336, 99.49999999999997158, -21.16602454745684270 ) ) ;
#3781 = ORIENTED_EDGE ( 'NONE', *, *, #8141, .T. ) ;
#3782 = DIRECTION ( 'NONE',  ( 1.000000000000000000, 0.000000000000000000, -0.000000000000000000 ) ) ;
#3783 = AXIS2_PLACEMENT_3D ( 'NONE', #1546, #10130, #10243 ) ;
#3784 = CARTESIAN_POINT ( 'NONE',  ( 19.39806930854667399, 3.349999998907525534, 19.39806930854668465 ) ) ;
#3785 =( NAMED_UNIT ( * ) PLANE_ANGLE_UNIT ( ) SI_UNIT ( $, .RADIAN. ) );
#3786 = EDGE_CURVE ( 'NONE', #2600, #3916, #1067, .T. ) ;
#3787 = DIRECTION ( 'NONE',  ( 0.000000000000000000, 0.000000000000000000, 1.000000000000000000 ) ) ;
#3788 = CARTESIAN_POINT ( 'NONE',  ( 11.18376618407356915, 0.9499999999999999556, -27.00000000000000355 ) ) ;
#3789 = FACE_OUTER_BOUND ( 'NONE', #7110, .T. ) ;
#3790 = ORIENTED_EDGE ( 'NONE', *, *, #8261, .F. ) ;
#3791 =( BOUNDED_CURVE ( )  B_SPLINE_CURVE ( 1, ( #3037, #8685 ),
 .UNSPECIFIED., .F., .F. ) 
 B_SPLINE_CURVE_WITH_KNOTS ( ( 2, 2 ),
 ( 0.000000000000000000, 1.000000000000000000 ),
 .UNSPECIFIED. ) 
 CURVE ( )  GEOMETRIC_REPRESENTATION_ITEM ( )  RATIONAL_B_SPLINE_CURVE ( ( 0.9401537613649495473, 0.9401537613649495473 ) ) 
 REPRESENTATION_ITEM ( '' )  );
#3792 = CARTESIAN_POINT ( 'NONE',  ( -16.57330815294036697, 99.99999999999997158, 15.84440382193293217 ) ) ;
#3793 = CARTESIAN_POINT ( 'NONE',  ( 8.117007248954752896, 99.50000000000001421, 20.40979824468519155 ) ) ;
#3794 = ORIENTED_EDGE ( 'NONE', *, *, #2370, .T. ) ;
#3795 = CARTESIAN_POINT ( 'NONE',  ( 2.256430356249999658, -4.040624999385483029, -1.302750673588581432 ) ) ;
#3796 = EDGE_LOOP ( 'NONE', ( #5326, #1888, #3883, #2068 ) ) ;
#3797 = ORIENTED_EDGE ( 'NONE', *, *, #4110, .F. ) ;
#3798 = CARTESIAN_POINT ( 'NONE',  ( 11.36312591709336850, 0.8999999989075253559, 27.43301269999999903 ) ) ;
#3799 = LINE ( 'NONE', #10239, #10070 ) ;
#3800 = EDGE_CURVE ( 'NONE', #7095, #2378, #1119, .T. ) ;
#3801 = CIRCLE ( 'NONE', #3618, 24.00000000000000355 ) ;
#3802 = CARTESIAN_POINT ( 'NONE',  ( -1.595409442497313560E-16, -1.715624999385482852, -2.605501347177161087 ) ) ;
#3803 = CARTESIAN_POINT ( 'NONE',  ( 0.000000000000000000, 85.00000000000000000, -7.500000000000000000 ) ) ;
#3804 = DIRECTION ( 'NONE',  ( 0.05376826219280737146, 0.000000000000000000, 0.9985534407235125975 ) ) ;
#3805 = CARTESIAN_POINT ( 'NONE',  ( 2.500000000000000000, -0.5812499987709658367, -1.443375672974064994 ) ) ;
#3806 = ORIENTED_EDGE ( 'NONE', *, *, #4909, .T. ) ;
#3807 = CYLINDRICAL_SURFACE ( 'NONE', #3139, 2.500000000000000000 ) ;
#3808 = CARTESIAN_POINT ( 'NONE',  ( 1.249999999999999334, -2.849999999999999645, -2.165063509461096825 ) ) ;
#3809 = ORIENTED_EDGE ( 'NONE', *, *, #4131, .F. ) ;
#3810 = DIRECTION ( 'NONE',  ( 0.000000000000000000, -1.000000000000000000, 0.000000000000000000 ) ) ;
#3811 = CARTESIAN_POINT ( 'NONE',  ( 2.256430356250000102, -1.715624999385482852, -2.763330213280484622E-16 ) ) ;
#3812 = PRODUCT_DEFINITION_FORMATION_WITH_SPECIFIED_SOURCE ( 'ANY', '', #3022, .NOT_KNOWN. ) ;
#3813 = ORIENTED_EDGE ( 'NONE', *, *, #2021, .T. ) ;
#3814 = CARTESIAN_POINT ( 'NONE',  ( -2.500000000000000000, -0.8812499987709659921, -1.443375672974064106 ) ) ;
#3815 = CARTESIAN_POINT ( 'NONE',  ( 8.429066232339796017, 100.0000000000000000, 19.67794530653910101 ) ) ;
#3816 = DIRECTION ( 'NONE',  ( -0.000000000000000000, 1.000000000000000000, -0.000000000000000000 ) ) ;
#3817 = DIRECTION ( 'NONE',  ( 0.000000000000000000, -1.000000000000000000, 0.000000000000000000 ) ) ;
#3818 = ORIENTED_EDGE ( 'NONE', *, *, #3693, .T. ) ;
#3819 = FACE_OUTER_BOUND ( 'NONE', #6950, .T. ) ;
#3820 = CARTESIAN_POINT ( 'NONE',  ( 27.43301270000000258, 0.3499999989075252005, 0.000000000000000000 ) ) ;
#3821 = VERTEX_POINT ( 'NONE', #3475 ) ;
#3822 = VECTOR ( 'NONE', #8896, 1000.000000000000000 ) ;
#3823 = CARTESIAN_POINT ( 'NONE',  ( -1.250000000000000222, -4.574999999999999289, -2.165063509461096825 ) ) ;
#3824 = ITEM_DEFINED_TRANSFORMATION ( 'NONE', 'NONE', #134,  #5055 ) ;
#3825 = CARTESIAN_POINT ( 'NONE',  ( 3.203979444200292015, 99.50000000000000000, -21.29640115293693725 ) ) ;
#3826 = CARTESIAN_POINT ( 'NONE',  ( 2.256430356249999658, -3.140624999385482674, -1.302750673588581432 ) ) ;
#3827 = CARTESIAN_POINT ( 'NONE',  ( -19.39806930854667755, 4.549999998907525267, -19.39806930854668110 ) ) ;
#3828 = CARTESIAN_POINT ( 'NONE',  ( -11.36312591709335962, 2.199999998907525622, -27.43301270000000258 ) ) ;
#3829 = CARTESIAN_POINT ( 'NONE',  ( 8.751508028230254865, 99.99999999999998579, 19.58480916780017722 ) ) ;
#3830 = CARTESIAN_POINT ( 'NONE',  ( 4.143207896384923039, 99.49999999999998579, -24.36264353342416911 ) ) ;
#3831 = CARTESIAN_POINT ( 'NONE',  ( 3.283294465904739390, 99.50000000000002842, -21.71066637097430885 ) ) ;
#3832 = EDGE_CURVE ( 'NONE', #10048, #4596, #2640, .T. ) ;
#3833 = CYLINDRICAL_SURFACE ( 'NONE', #4638, 2.500000000000000000 ) ;
#3834 = CARTESIAN_POINT ( 'NONE',  ( -2.256430356250000102, -1.940624999385482941, 0.000000000000000000 ) ) ;
#3835 = CARTESIAN_POINT ( 'NONE',  ( -21.94169572595625795, 99.50000000000000000, -9.715372641902229489 ) ) ;
#3836 = CARTESIAN_POINT ( 'NONE',  ( -1.595409442497313560E-16, -2.953124999385482674, -2.605501347177161087 ) ) ;
#3837 = CARTESIAN_POINT ( 'NONE',  ( 19.39806930854668110, 3.549999998907525267, -19.39806930854668110 ) ) ;
#3838 = VERTEX_POINT ( 'NONE', #8447 ) ;
#3839 = CARTESIAN_POINT ( 'NONE',  ( -15.29853103387017121, 99.50000000000001421, 14.98378122532347057 ) ) ;
#3840 = CARTESIAN_POINT ( 'NONE',  ( 11.18376618407356915, 2.549999999999999822, -27.00000000000000355 ) ) ;
#3841 = CARTESIAN_POINT ( 'NONE',  ( 9.404665101723468368, 100.0000000000000284, 20.17141824467128686 ) ) ;
#3842 = ORIENTED_EDGE ( 'NONE', *, *, #6044, .T. ) ;
#3843 = CARTESIAN_POINT ( 'NONE',  ( -27.00000000000000355, 2.799999999999999822, -3.306546357697854128E-15 ) ) ;
#3844 = FACE_OUTER_BOUND ( 'NONE', #6700, .T. ) ;
#3845 = ORIENTED_EDGE ( 'NONE', *, *, #8993, .T. ) ;
#3846 = CARTESIAN_POINT ( 'NONE',  ( -1.128215178124998497, -4.678124999385482319, 1.954126010382872147 ) ) ;
#3847 = ORIENTED_EDGE ( 'NONE', *, *, #3384, .T. ) ;
#3848 = CARTESIAN_POINT ( 'NONE',  ( 19.39806930854668110, 3.549999998907525267, -19.39806930854668110 ) ) ;
#3849 = CARTESIAN_POINT ( 'NONE',  ( 2.256430356250000102, -0.9281249993854827629, -2.763330213280484622E-16 ) ) ;
#3850 = CARTESIAN_POINT ( 'NONE',  ( -15.31787750341841559, 99.50000000000001421, 16.43551622900274722 ) ) ;
#3851 = CYLINDRICAL_SURFACE ( 'NONE', #10131, 23.99999999999999645 ) ;
#3852 =( BOUNDED_CURVE ( )  B_SPLINE_CURVE ( 2, ( #3820, #7570, #7621, #2133, #5271, #9301, #462, #7736, #3041, #6221, #2985, #9420, #7680, #4598, #3658, #7002, #622, #8469, #10206, #518, #5446, #9364, #9986, #6109, #5391, #8639, #6053, #4384, #3708, #408, #3603, #569, #8585, #6892, #6839, #8414, #10033, #2871, #6786, #10089, #2821, #6003, #9243, #9196, #6166, #2017, #5214, #2925, #1245, #2077, #5334, #4435, #1296, #8526, #1350, #6278, #7055, #7256, #10364, #6480, #3194, #4655, #39, #2348, #4705, #9570, #1612, #6330, #6375, #7846, #5547, #7897, #2403, #731, #10263, #3094, #833, #5597, #3923, #3242, #9474, #9524, #8738, #8001, #7109, #4807, #10309, #4026, #8689, #3144, #676, #2303, #2507, #6429, #1562, #7207, #4753, #5498, #9621, #5699, #1511 ),
 .UNSPECIFIED., .F., .F. ) 
 B_SPLINE_CURVE_WITH_KNOTS ( ( 3, 2, 2, 2, 2, 2, 2, 2, 2, 2, 2, 2, 2, 2, 2, 2, 2, 2, 2, 2, 2, 2, 2, 2, 2, 2, 2, 2, 2, 2, 2, 2, 2, 2, 2, 2, 2, 2, 2, 2, 2, 2, 2, 2, 2, 2, 2, 2, 2, 2, 3 ),
 ( 0.000000000000000000, 0.01785714285714285615, 0.03571428571428571230, 0.05357142857142856845, 0.07142857142857142461, 0.08928571428571428770, 0.1071428571428571369, 0.1250000000000000000, 0.1428571428571428492, 0.1607142857142857262, 0.1785714285714285754, 0.1964285714285714246, 0.2142857142857142738, 0.2321428571428571508, 0.2500000000000000000, 0.2678571428571428492, 0.2857142857142856984, 0.3035714285714285476, 0.3214285714285714524, 0.3392857142857143016, 0.3571428571428571508, 0.3750000000000000000, 0.3928571428571428492, 0.4107142857142856984, 0.4285714285714285476, 0.4464285714285714524, 0.4642857142857143016, 0.4821428571428571508, 0.5000000000000000000, 0.5178571428571429047, 0.5357142857142856984, 0.5535714285714286031, 0.5714285714285713969, 0.5892857142857143016, 0.6071428571428570953, 0.6250000000000000000, 0.6428571428571429047, 0.6607142857142856984, 0.6785714285714286031, 0.6964285714285715079, 0.7142857142857143016, 0.7321428571428570953, 0.7500000000000000000, 0.7678571428571429047, 0.7857142857142856984, 0.8035714285714286031, 0.8214285714285713969, 0.8392857142857143016, 0.8571428571428570953, 0.8750000000000000000, 0.8928571428571429047 ),
 .UNSPECIFIED. ) 
 CURVE ( )  GEOMETRIC_REPRESENTATION_ITEM ( )  RATIONAL_B_SPLINE_CURVE ( ( 1.000000000000000000, 0.9238795325112867385, 1.000000000000000000, 0.9238795325112867385, 1.000000000000000000, 0.9238795325112867385, 1.000000000000000000, 0.9238795325112867385, 1.000000000000000000, 0.9238795325112867385, 1.000000000000000000, 0.9238795325112867385, 1.000000000000000000, 0.9238795325112867385, 1.000000000000000000, 0.9238795325112867385, 1.000000000000000000, 0.9238795325112867385, 1.000000000000000000, 0.9238795325112867385, 1.000000000000000000, 0.9238795325112867385, 1.000000000000000000, 0.9238795325112867385, 1.000000000000000000, 0.9238795325112867385, 1.000000000000000000, 0.9238795325112867385, 1.000000000000000000, 0.9238795325112867385, 1.000000000000000000, 0.9238795325112867385, 1.000000000000000000, 0.9238795325112867385, 1.000000000000000000, 0.9238795325112867385, 1.000000000000000000, 0.9238795325112867385, 1.000000000000000000, 0.9238795325112867385, 1.000000000000000000, 0.9238795325112867385, 1.000000000000000000, 0.9238795325112867385, 1.000000000000000000, 0.9238795325112867385, 1.000000000000000000, 0.9238795325112867385, 1.000000000000000000, 0.9238795325112867385, 1.000000000000000000, 0.9238795325112867385, 1.000000000000000000, 0.9238795325112867385, 1.000000000000000000, 0.9238795325112867385, 1.000000000000000000, 0.9238795325112867385, 1.000000000000000000, 0.9238795325112867385, 1.000000000000000000, 0.9238795325112867385, 1.000000000000000000, 0.9238795325112867385, 1.000000000000000000, 0.9238795325112867385, 1.000000000000000000, 0.9238795325112867385, 1.000000000000000000, 0.9238795325112867385, 1.000000000000000000, 0.9238795325112867385, 1.000000000000000000, 0.9238795325112867385, 1.000000000000000000, 0.9238795325112867385, 1.000000000000000000, 0.9238795325112867385, 1.000000000000000000, 0.9238795325112867385, 1.000000000000000000, 0.9238795325112867385, 1.000000000000000000, 0.9238795325112867385, 1.000000000000000000, 0.9238795325112867385, 1.000000000000000000, 0.9238795325112867385, 1.000000000000000000, 0.9238795325112867385, 1.000000000000000000, 0.9238795325112867385, 1.000000000000000000, 0.9238795325112867385, 1.000000000000000000, 0.9238795325112867385, 1.000000000000000000, 0.9238795325112867385, 1.000000000000000000, 0.9238795325112867385, 1.000000000000000000 ) ) 
 REPRESENTATION_ITEM ( '' )  );
#3853 = EDGE_CURVE ( 'NONE', #486, #84, #7440, .T. ) ;
#3854 = EDGE_CURVE ( 'NONE', #10177, #10048, #9078, .T. ) ;
#3855 = CARTESIAN_POINT ( 'NONE',  ( 5.302876193624534821E-16, -1.181249998770965703, 2.886751345948128655 ) ) ;
#3856 = CARTESIAN_POINT ( 'NONE',  ( 4.504418077186241653, 100.0000000000000426, -21.31258943653750393 ) ) ;
#3857 = FACE_OUTER_BOUND ( 'NONE', #6081, .T. ) ;
#3858 = ORIENTED_EDGE ( 'NONE', *, *, #1949, .T. ) ;
#3859 = CARTESIAN_POINT ( 'NONE',  ( 8.536201443755420115, 99.50000000000002842, 19.63502355897212581 ) ) ;
#3860 = CARTESIAN_POINT ( 'NONE',  ( -1.128215178124998497, -0.9656249993854828517, 1.954126010382872147 ) ) ;
#3861 = EDGE_LOOP ( 'NONE', ( #5742, #783, #9448, #1942 ) ) ;
#3862 = DIRECTION ( 'NONE',  ( 0.000000000000000000, -1.000000000000000000, 0.000000000000000000 ) ) ;
#3863 = CIRCLE ( 'NONE', #5186, 2.500000000000000000 ) ;
#3864 = FACE_OUTER_BOUND ( 'NONE', #1272, .T. ) ;
#3865 = PRESENTATION_STYLE_ASSIGNMENT (( #5544 ) ) ;
#3866 = CARTESIAN_POINT ( 'NONE',  ( -22.12191435419165941, 99.50000000000001421, -9.834338183724410598 ) ) ;
#3867 = ORIENTED_EDGE ( 'NONE', *, *, #428, .T. ) ;
#3868 = CARTESIAN_POINT ( 'NONE',  ( -15.34161522349497808, 99.99999999999998579, 15.37783959465231121 ) ) ;
#3869 = CARTESIAN_POINT ( 'NONE',  ( 8.757234875838378230, 100.0000000000000000, 19.92790116963689329 ) ) ;
#3870 = EDGE_LOOP ( 'NONE', ( #136, #5921, #330, #9703 ) ) ;
#3871 = SURFACE_SIDE_STYLE ('',( #678 ) ) ;
#3872 = DIRECTION ( 'NONE',  ( 0.000000000000000000, -1.000000000000000000, 0.000000000000000000 ) ) ;
#3873 = CARTESIAN_POINT ( 'NONE',  ( 2.256430356250000546, -5.015624999385482674, 1.302750673588579877 ) ) ;
#3874 = CARTESIAN_POINT ( 'NONE',  ( 4.909381318607588973, 99.50000000000000000, -23.54377677363417121 ) ) ;
#3875 = CARTESIAN_POINT ( 'NONE',  ( 19.39806930854668110, 1.249999998907525223, -19.39806930854668110 ) ) ;
#3876 = CARTESIAN_POINT ( 'NONE',  ( -15.32348647777738826, 99.99999999999997158, 15.39505148541300450 ) ) ;
#3877 = VECTOR ( 'NONE', #3810, 1000.000000000000000 ) ;
#3878 = CARTESIAN_POINT ( 'NONE',  ( 3.810791133452845703, 99.50000000000005684, -24.33305202239136733 ) ) ;
#3879 = CARTESIAN_POINT ( 'NONE',  ( -19.46743691185369585, 100.0000000000000000, -8.912588186774021537 ) ) ;
#3880 = CARTESIAN_POINT ( 'NONE',  ( 21.43339342948717885, 99.50000000000000000, -1.392427884615384803 ) ) ;
#3881 = CARTESIAN_POINT ( 'NONE',  ( -2.256430356250000102, -2.428124999385482763, -1.302750673588580321 ) ) ;
#3882 = CARTESIAN_POINT ( 'NONE',  ( 3.739209042966563867, 100.0000000000000000, -21.42288334414699236 ) ) ;
#3883 = ORIENTED_EDGE ( 'NONE', *, *, #1844, .T. ) ;
#3884 = ORIENTED_EDGE ( 'NONE', *, *, #1844, .F. ) ;
#3885 = CARTESIAN_POINT ( 'NONE',  ( -1.128215178125000273, -2.015624999385483118, -1.954126010382871259 ) ) ;
#3886 = CARTESIAN_POINT ( 'NONE',  ( 1.679787559701184688E-15, 4.449999998907525622, -27.43301270000000258 ) ) ;
#3887 =( NAMED_UNIT ( * ) PLANE_ANGLE_UNIT ( ) SI_UNIT ( $, .RADIAN. ) );
#3888 = CARTESIAN_POINT ( 'NONE',  ( -15.42740294075255925, 99.50000000000000000, 14.91894146668702348 ) ) ;
#3889 = VECTOR ( 'NONE', #1869, 1000.000000000000000 ) ;
#3890 = EDGE_CURVE ( 'NONE', #10071, #3238, #4360, .T. ) ;
#3891 = CARTESIAN_POINT ( 'NONE',  ( -27.00000000000000355, 1.950000000000000400, -11.18376618407357093 ) ) ;
#3892 = CARTESIAN_POINT ( 'NONE',  ( 3.000000000000000000, -15.00000000000000000, 1.732050807568879192 ) ) ;
#3893 = ORIENTED_EDGE ( 'NONE', *, *, #7153, .F. ) ;
#3894 = CARTESIAN_POINT ( 'NONE',  ( -16.56356094049941419, 99.99999999999994316, 15.77213757552179629 ) ) ;
#3895 = CARTESIAN_POINT ( 'NONE',  ( -15.62070810370258833, 100.0000000000000000, 16.62245103965875970 ) ) ;
#3896 = CARTESIAN_POINT ( 'NONE',  ( -1.128215178125000273, -4.828124999385481786, -1.954126010382871259 ) ) ;
#3897 = EDGE_LOOP ( 'NONE', ( #7154, #8892, #4802, #4225 ) ) ;
#3898 = CIRCLE ( 'NONE', #1036, 17.50000000000000355 ) ;
#3899 = CARTESIAN_POINT ( 'NONE',  ( 19.39806930854667399, 2.549999998907525267, 19.39806930854668465 ) ) ;
#3900 = CARTESIAN_POINT ( 'NONE',  ( -21.91899880027261460, 99.50000000000000000, -9.705014769524845875 ) ) ;
#3901 = CARTESIAN_POINT ( 'NONE',  ( -2.256430356249998770, -1.565624999385482941, 1.302750673588581876 ) ) ;
#3902 = CARTESIAN_POINT ( 'NONE',  ( 2.928963527206765338, 99.99999999999997158, -23.52685633767685758 ) ) ;
#3903 = EDGE_CURVE ( 'NONE', #2398, #827, #10035, .T. ) ;
#3904 = ORIENTED_EDGE ( 'NONE', *, *, #8426, .F. ) ;
#3905 = CARTESIAN_POINT ( 'NONE',  ( 4.405197143102897783, 99.49999999999995737, -21.72932741277565682 ) ) ;
#3906 = AXIS2_PLACEMENT_3D ( 'NONE', #3532, #8347, #4318 ) ;
#3907 = ORIENTED_EDGE ( 'NONE', *, *, #4748, .F. ) ;
#3908 = CARTESIAN_POINT ( 'NONE',  ( -2.499999999999999556, -1.256249998770965659, 1.443375672974065882 ) ) ;
#3909 = ORIENTED_EDGE ( 'NONE', *, *, #2818, .F. ) ;
#3910 = CARTESIAN_POINT ( 'NONE',  ( 4.457146071884139360, 100.0000000000000284, -24.28472590373185724 ) ) ;
#3911 = CARTESIAN_POINT ( 'NONE',  ( -15.58193289918752278, 99.50000000000000000, 16.98546238400348329 ) ) ;
#3912 = EDGE_CURVE ( 'NONE', #3208, #6241, #3578, .T. ) ;
#3913 = DIRECTION ( 'NONE',  ( 1.000000000000000000, 0.000000000000000000, 0.000000000000000000 ) ) ;
#3914 = CARTESIAN_POINT ( 'NONE',  ( -1.128215178124998497, -1.415624999385482807, 1.954126010382872147 ) ) ;
#3915 = EDGE_CURVE ( 'NONE', #4694, #7282, #5312, .T. ) ;
#3916 = VERTEX_POINT ( 'NONE', #3639 ) ;
#3917 = CARTESIAN_POINT ( 'NONE',  ( -22.21584973381871464, 100.0000000000000142, -9.938501092090024969 ) ) ;
#3918 = CARTESIAN_POINT ( 'NONE',  ( 9.666415885916139317, 100.0000000000000142, 19.95264712196244261 ) ) ;
#3919 = FILL_AREA_STYLE ('',( #4855 ) ) ;
#3920 = CARTESIAN_POINT ( 'NONE',  ( -2.500000000000000000, -3.543749998770965526, 0.000000000000000000 ) ) ;
#3921 = ORIENTED_EDGE ( 'NONE', *, *, #6836, .T. ) ;
#3922 = CARTESIAN_POINT ( 'NONE',  ( -14.75894607058735630, 99.50000000000002842, 15.77473972644577849 ) ) ;
#3923 = CARTESIAN_POINT ( 'NONE',  ( 19.39806930854667399, 4.249999998907525445, 19.39806930854668465 ) ) ;
#3924 = ORIENTED_EDGE ( 'NONE', *, *, #103, .T. ) ;
#3925 = CARTESIAN_POINT ( 'NONE',  ( 1.249999999999999334, -4.649999999999999467, -2.165063509461096825 ) ) ;
#3926 = CONTEXT_DEPENDENT_SHAPE_REPRESENTATION ( #1390, #9613 ) ;
#3927 = CARTESIAN_POINT ( 'NONE',  ( -1.250000000000000222, -0.4687499987709658478, -2.165063509461096825 ) ) ;
#3928 = CARTESIAN_POINT ( 'NONE',  ( -2.256430356250000102, -5.203124999385482674, 0.000000000000000000 ) ) ;
#3929 = DIRECTION ( 'NONE',  ( 0.000000000000000000, 1.000000000000000000, 0.000000000000000000 ) ) ;
#3930 = CARTESIAN_POINT ( 'NONE',  ( -19.39806930854668465, 4.849999998907525978, 19.39806930854667755 ) ) ;
#3931 = LINE ( 'NONE', #8698, #1917 ) ;
#3932 = VECTOR ( 'NONE', #3058, 1000.000000000000000 ) ;
#3933 = CARTESIAN_POINT ( 'NONE',  ( 3.735769352376668184, 99.49999999999998579, -24.30643046864489420 ) ) ;
#3934 = DIRECTION ( 'NONE',  ( -0.7071067811865474617, 0.000000000000000000, 0.7071067811865476838 ) ) ;
#3935 = B_SPLINE_SURFACE_WITH_KNOTS ( 'NONE', 3, 1, ( 
 ( #2780, #7585 ),
 ( #4505, #423 ),
 ( #7698, #3620 ),
 ( #8602, #9436 ),
 ( #2363, #5463 ),
 ( #5514, #6181 ),
 ( #2314, #1425 ),
 ( #7807, #10222 ),
 ( #5409, #9379 ),
 ( #9491, #5611 ),
 ( #3780, #9539 ),
 ( #8653, #3938 ),
 ( #6292, #2207 ),
 ( #4613, #3161 ),
 ( #1475, #3005 ),
 ( #6344, #3207 ),
 ( #2264, #4670 ),
 ( #10276, #7861 ),
 ( #5560, #6967 ) ),
 .UNSPECIFIED., .F., .F., .F.,
 ( 4, 1, 1, 1, 1, 1, 1, 1, 1, 1, 1, 1, 1, 1, 1, 1, 4 ),
 ( 2, 2 ),
 ( 0.000000000000000000, 0.07315862907712983310, 0.1430989967074559055, 0.2105333571262071879, 0.2759142635903734653, 0.3397077151413689933, 0.4013946392018796772, 0.4627937533375801049, 0.5237250720276656057, 0.5836284080752294212, 0.6425725562371763511, 0.7010486867616194662, 0.7591976973140022178, 0.8177727706511607186, 0.8769111530050104353, 0.9375229829315941954, 1.000000000000000000 ),
 ( 0.000000000000000000, 1.000000000000000000 ),
 .UNSPECIFIED. ) ;
#3936 = CARTESIAN_POINT ( 'NONE',  ( -16.07368679829020763, 100.0000000000000000, 17.11560437002838952 ) ) ;
#3937 = CARTESIAN_POINT ( 'NONE',  ( -2.256430356249998770, -2.803124999385482763, 1.302750673588581876 ) ) ;
#3938 = CARTESIAN_POINT ( 'NONE',  ( 4.200543313440712190, 100.0000000000000000, -21.13206004899810608 ) ) ;
#3939 = VERTEX_POINT ( 'NONE', #6818 ) ;
#3940 = CARTESIAN_POINT ( 'NONE',  ( 2.256430356250000546, -3.103124999385482585, 1.302750673588579877 ) ) ;
#3941 = CARTESIAN_POINT ( 'NONE',  ( 11.36312591709336850, 4.099999998907525089, 27.43301269999999903 ) ) ;
#3942 = CARTESIAN_POINT ( 'NONE',  ( 0.000000000000000000, 0.000000000000000000, -2.500000000000000000 ) ) ;
#3943 = CARTESIAN_POINT ( 'NONE',  ( -27.00000000000000355, 1.200000000000000178, -3.306546357697854128E-15 ) ) ;
#3944 = CARTESIAN_POINT ( 'NONE',  ( 3.411785164761435674, 100.0000000000000000, -22.76693382491622231 ) ) ;
#3945 = ORIENTED_EDGE ( 'NONE', *, *, #3581, .F. ) ;
#3946 = VECTOR ( 'NONE', #9820, 1000.000000000000000 ) ;
#3947 = LINE ( 'NONE', #2530, #6641 ) ;
#3948 = CARTESIAN_POINT ( 'NONE',  ( 8.122452352567329115, 99.50000000000000000, 21.04970292111833530 ) ) ;
#3949 = CARTESIAN_POINT ( 'NONE',  ( 1.128215178125001161, -3.253124999385482496, 1.954126010382870815 ) ) ;
#3950 = CARTESIAN_POINT ( 'NONE',  ( 2.939152317953647500E-15, 71.18660744634364335, -23.99999999999999645 ) ) ;
#3951 = EDGE_CURVE ( 'NONE', #1383, #4882, #974, .T. ) ;
#3952 = B_SPLINE_CURVE_WITH_KNOTS ( 'NONE', 3,
 ( #9431, #10161, #9203, #7632, #3829, #6175, #6013, #9315, #1418, #472, #4553, #1360, #2882, #6796, #3048, #6119, #7013, #2937, #1254 ),
 .UNSPECIFIED., .F., .F.,
 ( 4, 1, 1, 1, 1, 1, 1, 1, 1, 1, 1, 1, 1, 1, 1, 1, 4 ),
 ( 0.000000000000000000, 0.07024023345195122559, 0.1375772235014411093, 0.2026681864156774648, 0.2655894380381068620, 0.3279415367477454546, 0.3896445486312665740, 0.4521557380645868096, 0.5154465764363311830, 0.5785479733725392704, 0.6397241484143471046, 0.6996998702489094502, 0.7590513234224176564, 0.8180896689983322423, 0.8773873076253557723, 0.9378402036119877216, 1.000000000000000000 ),
 .UNSPECIFIED. ) ;
#3953 = CARTESIAN_POINT ( 'NONE',  ( -19.39806930854667755, 2.949999998907525178, -19.39806930854668110 ) ) ;
#3954 = CARTESIAN_POINT ( 'NONE',  ( 1.250000000000001110, -4.293749998770965526, 2.165063509461096380 ) ) ;
#3955 = CARTESIAN_POINT ( 'NONE',  ( -22.57971655928959365, 99.50000000000000000, -10.84768434062017839 ) ) ;
#3956 = CARTESIAN_POINT ( 'NONE',  ( -1.128215178125000273, -3.028124999385482408, -1.954126010382871259 ) ) ;
#3957 = FACE_OUTER_BOUND ( 'NONE', #8668, .T. ) ;
#3958 = CARTESIAN_POINT ( 'NONE',  ( -16.76168403648438243, 99.50000000000002842, 16.44483764528499847 ) ) ;
#3959 = CARTESIAN_POINT ( 'NONE',  ( 27.00000000000000355, 4.649999997815049468, -11.18376618407356915 ) ) ;
#3960 = CARTESIAN_POINT ( 'NONE',  ( -1.767625397874844694E-16, -3.206249998770965615, -2.886751345948128655 ) ) ;
#3961 = EDGE_CURVE ( 'NONE', #8911, #3601, #5295, .T. ) ;
#3962 = TOROIDAL_SURFACE ( 'NONE', #5960, 23.82500000000000284, 1.324999999999999956 ) ;
#3963 = CARTESIAN_POINT ( 'NONE',  ( 4.523042264738025509, 100.0000000000000284, -24.25177047807976294 ) ) ;
#3964 = CARTESIAN_POINT ( 'NONE',  ( 0.000000000000000000, 87.00000000000001421, 0.000000000000000000 ) ) ;
#3965 = CARTESIAN_POINT ( 'NONE',  ( 0.000000000000000000, 72.50000000000001421, 0.000000000000000000 ) ) ;
#3966 = CARTESIAN_POINT ( 'NONE',  ( 1.128215178124999607, -3.890624999385482674, -1.954126010382871259 ) ) ;
#3967 = ORIENTED_EDGE ( 'NONE', *, *, #1977, .F. ) ;
#3968 = ORIENTED_EDGE ( 'NONE', *, *, #7539, .F. ) ;
#3969 = CARTESIAN_POINT ( 'NONE',  ( -22.33391032228853490, 100.0000000000000284, -10.55243757774135993 ) ) ;
#3970 = AXIS2_PLACEMENT_3D ( 'NONE', #1664, #1561, #6374 ) ;
#3971 = ORIENTED_EDGE ( 'NONE', *, *, #8252, .F. ) ;
#3972 = FILL_AREA_STYLE_COLOUR ( '', #688 ) ;
#3973 = CARTESIAN_POINT ( 'NONE',  ( -22.25406130147340633, 99.50000000000002842, -9.998337329044998611 ) ) ;
#3974 = CARTESIAN_POINT ( 'NONE',  ( 11.18376618407357626, 2.849999997815050978, 27.00000000000000000 ) ) ;
#3975 = CARTESIAN_POINT ( 'NONE',  ( 9.502908418173033667, 100.0000000000000000, 20.32929868008965002 ) ) ;
#3976 = ORIENTED_EDGE ( 'NONE', *, *, #1064, .F. ) ;
#3977 = CARTESIAN_POINT ( 'NONE',  ( 1.250000000000001110, -3.449999999999999289, 2.165063509461096380 ) ) ;
#3978 =( GEOMETRIC_REPRESENTATION_CONTEXT ( 3 ) GLOBAL_UNCERTAINTY_ASSIGNED_CONTEXT ( ( #8534 ) ) GLOBAL_UNIT_ASSIGNED_CONTEXT ( ( #9367, #2989, #3606 ) ) REPRESENTATION_CONTEXT ( 'NONE', 'WORKASPACE' ) );
#3979 = CARTESIAN_POINT ( 'NONE',  ( 3.207057600658871355, 100.0000000000000000, -22.07913334414698880 ) ) ;
#3980 = CARTESIAN_POINT ( 'NONE',  ( 1.128215178125001161, -4.603124999385482141, 1.954126010382870815 ) ) ;
#3981 = CARTESIAN_POINT ( 'NONE',  ( -21.07742585509981126, 99.49999999999998579, -10.85999754779651383 ) ) ;
#3982 = CARTESIAN_POINT ( 'NONE',  ( -19.39806930854667755, 4.649999998907525800, -19.39806930854668110 ) ) ;
#3983 = CARTESIAN_POINT ( 'NONE',  ( -20.63666786535793207, 99.99999999999998579, -10.16306733409737717 ) ) ;
#3984 = EDGE_LOOP ( 'NONE', ( #9941, #4463 ) ) ;
#3985 = DIRECTION ( 'NONE',  ( 0.000000000000000000, 1.000000000000000000, 0.000000000000000000 ) ) ;
#3986 = CARTESIAN_POINT ( 'NONE',  ( -15.98323291606820362, 99.49999999999998579, 16.64087298452848884 ) ) ;
#3987 = EDGE_CURVE ( 'NONE', #9561, #5726, #2024, .T. ) ;
#3988 = CARTESIAN_POINT ( 'NONE',  ( 4.835062408351179286, 100.0000000000000000, -21.79588013901878440 ) ) ;
#3989 = AXIS2_PLACEMENT_3D ( 'NONE', #4608, #7801, #2148 ) ;
#3990 = CARTESIAN_POINT ( 'NONE',  ( -1.128215178125000273, -4.265624999385482674, -1.954126010382871259 ) ) ;
#3991 = CARTESIAN_POINT ( 'NONE',  ( -22.05573893622344173, 99.50000000000000000, -9.391591294897233766 ) ) ;
#3992 = ORIENTED_EDGE ( 'NONE', *, *, #7468, .F. ) ;
#3993 = CARTESIAN_POINT ( 'NONE',  ( -2.256430356249999214, -2.353124999385482585, 1.302750673588581876 ) ) ;
#3994 = CARTESIAN_POINT ( 'NONE',  ( 19.39806930854668110, 4.349999998907525089, -19.39806930854668110 ) ) ;
#3995 = SURFACE_STYLE_USAGE ( .BOTH. , #2419 ) ;
#3996 = DIRECTION ( 'NONE',  ( 0.000000000000000000, -1.000000000000000000, 0.000000000000000000 ) ) ;
#3997 = CARTESIAN_POINT ( 'NONE',  ( -27.00000000000000355, 4.350000000000000533, -11.18376618407357093 ) ) ;
#3998 = CIRCLE ( 'NONE', #9801, 1.324999999999999956 ) ;
#3999 = CARTESIAN_POINT ( 'NONE',  ( 3.298672054714395063, 99.50000000000001421, -22.72039518595936869 ) ) ;
#4000 = ORIENTED_EDGE ( 'NONE', *, *, #2556, .T. ) ;
#4001 = CARTESIAN_POINT ( 'NONE',  ( 8.117007248954752896, 100.0000000000000142, 20.40979824468519155 ) ) ;
#4002 = VERTEX_POINT ( 'NONE', #6652 ) ;
#4003 = CARTESIAN_POINT ( 'NONE',  ( 2.256430356250000102, -4.078124999385482674, -2.763330213280484622E-16 ) ) ;
#4004 = ORIENTED_EDGE ( 'NONE', *, *, #8242, .T. ) ;
#4005 = CARTESIAN_POINT ( 'NONE',  ( -5.039362679103552881E-15, 4.049999998907525267, 27.43301270000000258 ) ) ;
#4006 = CARTESIAN_POINT ( 'NONE',  ( 4.241330131419338123, 99.49999999999998579, -24.68798891778770965 ) ) ;
#4007 = CARTESIAN_POINT ( 'NONE',  ( -27.00000000000000355, 0.9999999978150503344, -3.306546357697854128E-15 ) ) ;
#4008 = CARTESIAN_POINT ( 'NONE',  ( -1.595409442497313560E-16, -4.415624999385482141, -2.605501347177161087 ) ) ;
#4009 = LINE ( 'NONE', #5682, #3228 ) ;
#4010 = CARTESIAN_POINT ( 'NONE',  ( -16.62994343074595349, 99.49999999999998579, 15.18287566599475191 ) ) ;
#4011 = PLANE ( 'NONE',  #1093 ) ;
#4012 = ORIENTED_EDGE ( 'NONE', *, *, #8191, .F. ) ;
#4013 = CARTESIAN_POINT ( 'NONE',  ( 1.249999999999999334, -3.243749998770965259, -2.165063509461096825 ) ) ;
#4014 = CARTESIAN_POINT ( 'NONE',  ( 4.793167276645844410, 99.99999999999998579, -21.69837440717521204 ) ) ;
#4015 = ADVANCED_BREP_SHAPE_REPRESENTATION ( '', ( #9927, #5055 ), #7565 ) ;
#4016 = CARTESIAN_POINT ( 'NONE',  ( -16.35834224700816009, 99.50000000000000000, 16.43761959438736397 ) ) ;
#4017 = CARTESIAN_POINT ( 'NONE',  ( -15.07178375341841559, 100.0000000000000142, 15.16157792772069968 ) ) ;
#4018 = CARTESIAN_POINT ( 'NONE',  ( 2.256430356250000546, -4.453124999385482674, 1.302750673588579877 ) ) ;
#4019 = EDGE_CURVE ( 'NONE', #8640, #6767, #6384, .T. ) ;
#4020 = B_SPLINE_SURFACE_WITH_KNOTS ( 'NONE', 3, 1, ( 
 ( #861, #5901 ),
 ( #2766, #252 ),
 ( #4383, #5956 ),
 ( #9149, #7569 ),
 ( #4834, #3439 ),
 ( #1966, #406 ),
 ( #3602, #9985 ),
 ( #9825, #6785 ),
 ( #6631, #2820 ),
 ( #2660, #3265 ),
 ( #7233, #8812 ) ),
 .UNSPECIFIED., .F., .F., .F.,
 ( 4, 1, 1, 1, 1, 1, 1, 1, 4 ),
 ( 2, 2 ),
 ( 0.000000000000000000, 0.1514666391271576040, 0.2940212016997327260, 0.4289076436562640482, 0.5568069201790899481, 0.6759213874835566793, 0.7888117551744765477, 0.8972989960681465593, 1.000000000000000000 ),
 ( 0.000000000000000000, 1.000000000000000000 ),
 .UNSPECIFIED. ) ;
#4021 = ORIENTED_EDGE ( 'NONE', *, *, #2423, .F. ) ;
#4022 = CARTESIAN_POINT ( 'NONE',  ( 0.000000000000000000, 0.000000000000000000, -2.500000000000000000 ) ) ;
#4023 = CARTESIAN_POINT ( 'NONE',  ( 0.000000000000000000, 97.50000000000000000, 0.000000000000000000 ) ) ;
#4024 = CARTESIAN_POINT ( 'NONE',  ( -16.40919047799676989, 99.50000000000000000, 16.38364531277195013 ) ) ;
#4025 = CARTESIAN_POINT ( 'NONE',  ( 0.000000000000000000, 87.00000000000001421, 0.000000000000000000 ) ) ;
#4026 = CARTESIAN_POINT ( 'NONE',  ( -27.43301270000000258, 4.699999998907525622, -11.36312591709336317 ) ) ;
#4027 = VERTEX_POINT ( 'NONE', #6753 ) ;
#4028 = CARTESIAN_POINT ( 'NONE',  ( 3.375079225685456041, 99.50000000000000000, -22.79123997459842954 ) ) ;
#4029 = CARTESIAN_POINT ( 'NONE',  ( 4.100286767325537873, 100.0000000000000000, -22.51382885696750336 ) ) ;
#4030 = CARTESIAN_POINT ( 'NONE',  ( -2.256430356250000102, -3.440624999385482496, -1.302750673588580321 ) ) ;
#4031 = CARTESIAN_POINT ( 'NONE',  ( -20.88772068548257366, 99.50000000000001421, -11.14739719174079546 ) ) ;
#4032 = CARTESIAN_POINT ( 'NONE',  ( 27.43301270000000258, 5.149999998907525800, 0.000000000000000000 ) ) ;
#4033 = UNCERTAINTY_MEASURE_WITH_UNIT (LENGTH_MEASURE( 1.000000000000000082E-05 ), #5013, 'distance_accuracy_value', 'NONE');
#4034 = CARTESIAN_POINT ( 'NONE',  ( -15.22320097062094568, 99.99999999999998579, 16.32303119091969634 ) ) ;
#4035 = DIRECTION ( 'NONE',  ( 0.000000000000000000, 1.000000000000000000, 0.000000000000000000 ) ) ;
#4036 = CARTESIAN_POINT ( 'NONE',  ( -16.24524625128438515, 99.50000000000002842, 16.53274063862002308 ) ) ;
#4037 = CARTESIAN_POINT ( 'NONE',  ( -22.67573144110267336, 100.0000000000000142, -10.14737752305977381 ) ) ;
#4038 = CARTESIAN_POINT ( 'NONE',  ( 2.256430356250000102, -4.415624999385482141, -2.763330213280484622E-16 ) ) ;
#4039 = CARTESIAN_POINT ( 'NONE',  ( 9.723125805078051798, 100.0000000000000000, 21.50134635983626907 ) ) ;
#4040 = VERTEX_POINT ( 'NONE', #1105 ) ;
#4041 = CARTESIAN_POINT ( 'NONE',  ( 1.128215178124999607, -1.190624999385482941, -1.954126010382871259 ) ) ;
#4042 = CARTESIAN_POINT ( 'NONE',  ( 19.39806930854667399, 4.949999998907525622, 19.39806930854668465 ) ) ;
#4043 = EDGE_CURVE ( 'NONE', #9118, #4569, #4298, .T. ) ;
#4044 = DIRECTION ( 'NONE',  ( 0.000000000000000000, 0.000000000000000000, -1.000000000000000000 ) ) ;
#4045 = EDGE_CURVE ( 'NONE', #3613, #7425, #2917, .T. ) ;
#4046 = CARTESIAN_POINT ( 'NONE',  ( -19.09188309203678813, 2.900000000000000355, 19.09188309203678457 ) ) ;
#4047 = CARTESIAN_POINT ( 'NONE',  ( 0.6698729810778112359, -3.226346188203299992, -2.499999999999996447 ) ) ;
#4048 = ORIENTED_EDGE ( 'NONE', *, *, #8265, .T. ) ;
#4049 = CARTESIAN_POINT ( 'NONE',  ( 0.000000000000000000, 0.000000000000000000, 0.000000000000000000 ) ) ;
#4050 = DIRECTION ( 'NONE',  ( -0.000000000000000000, 1.000000000000000000, -0.000000000000000000 ) ) ;
#4051 = DIRECTION ( 'NONE',  ( 0.000000000000000000, 0.000000000000000000, -1.000000000000000000 ) ) ;
#4052 = CARTESIAN_POINT ( 'NONE',  ( 0.6698729810778112359, -5.026346188203299370, -2.499999999999996447 ) ) ;
#4053 = CARTESIAN_POINT ( 'NONE',  ( -27.43301270000000258, 1.399999998907525134, -11.36312591709336317 ) ) ;
#4054 = CARTESIAN_POINT ( 'NONE',  ( -4.959819536546781389E-15, 2.200000000000000178, 27.00000000000000355 ) ) ;
#4055 = VECTOR ( 'NONE', #4095, 1000.000000000000000 ) ;
#4056 = CARTESIAN_POINT ( 'NONE',  ( -22.33589105551819642, 99.50000000000002842, -11.18147695539509812 ) ) ;
#4057 = CARTESIAN_POINT ( 'NONE',  ( 4.786228327491940187E-16, -2.840624999385482852, 2.605501347177161087 ) ) ;
#4058 = CARTESIAN_POINT ( 'NONE',  ( -16.52157078939288937, 99.99999999999998579, 16.20087177393598665 ) ) ;
#4059 = FACE_OUTER_BOUND ( 'NONE', #41, .T. ) ;
#4060 = CARTESIAN_POINT ( 'NONE',  ( 0.000000000000000000, 85.00000000000000000, 0.000000000000000000 ) ) ;
#4061 = VECTOR ( 'NONE', #8403, 1000.000000000000114 ) ;
#4062 = CARTESIAN_POINT ( 'NONE',  ( -2.500000000000000000, -2.643749998770965615, 0.000000000000000000 ) ) ;
#4063 = CARTESIAN_POINT ( 'NONE',  ( 4.723706824522782455, 99.50000000000000000, -24.08630974238606370 ) ) ;
#4064 = CARTESIAN_POINT ( 'NONE',  ( -15.89341924297059094, 99.50000000000001421, 17.07725933521297890 ) ) ;
#4065 = SHAPE_REPRESENTATION ( 'Reservoir Tank', ( #5055 ), #8584 ) ;
#4066 = PLANE ( 'NONE',  #1538 ) ;
#4067 = CARTESIAN_POINT ( 'NONE',  ( -2.256430356250000102, -3.740624999385482763, 0.000000000000000000 ) ) ;
#4068 = MECHANICAL_DESIGN_GEOMETRIC_PRESENTATION_REPRESENTATION (  '', ( #7237 ), #7083 ) ;
#4069 = CARTESIAN_POINT ( 'NONE',  ( -22.34945848979098670, 100.0000000000000284, -10.27225542379191481 ) ) ;
#4070 = APPLICATION_CONTEXT ( 'automotive_design' ) ;
#4071 = CARTESIAN_POINT ( 'NONE',  ( 0.000000000000000000, 70.00000000000000000, 0.000000000000000000 ) ) ;
#4072 = CARTESIAN_POINT ( 'NONE',  ( -21.94169572595625795, 99.50000000000000000, -9.715372641902229489 ) ) ;
#4073 = CARTESIAN_POINT ( 'NONE',  ( -11.18376618407356737, 2.449999997815050623, -27.00000000000000355 ) ) ;
#4074 = CARTESIAN_POINT ( 'NONE',  ( 9.304660012616079001, 100.0000000000000000, 20.07619068507570859 ) ) ;
#4075 = VERTEX_POINT ( 'NONE', #2783 ) ;
#4076 = ADVANCED_FACE ( 'NONE', ( #221 ), #3107, .T. ) ;
#4077 = DIRECTION ( 'NONE',  ( 0.000000000000000000, 1.000000000000000000, 0.000000000000000000 ) ) ;
#4078 = CARTESIAN_POINT ( 'NONE',  ( -21.03403678956047074, 100.0000000000000142, -10.80451401317004922 ) ) ;
#4079 = CARTESIAN_POINT ( 'NONE',  ( -2.256430356249999658, -5.226765559567681407, -0.8212734853698877568 ) ) ;
#4080 = CARTESIAN_POINT ( 'NONE',  ( -20.61566945723384592, 100.0000000000000000, -10.83949095114527594 ) ) ;
#4081 = CARTESIAN_POINT ( 'NONE',  ( 27.43301269999999548, 4.299999998907526155, 11.36312591709337738 ) ) ;
#4082 = CARTESIAN_POINT ( 'NONE',  ( -15.13293277027690209, 99.50000000000000000, 16.13104881108577970 ) ) ;
#4083 = CARTESIAN_POINT ( 'NONE',  ( 27.00000000000000355, 3.849999997815050534, -11.18376618407356915 ) ) ;
#4084 = CARTESIAN_POINT ( 'NONE',  ( 3.673732336774000018, 100.0000000000000000, -21.43557726391590279 ) ) ;
#4085 = CARTESIAN_POINT ( 'NONE',  ( -22.69331084068295112, 99.99999999999998579, -10.43328931840349050 ) ) ;
#4086 = CARTESIAN_POINT ( 'NONE',  ( 2.256430356249999658, -3.928124999385482319, -1.302750673588581432 ) ) ;
#4087 = CARTESIAN_POINT ( 'NONE',  ( 9.873655262861264603, 100.0000000000000000, 20.34710108723753308 ) ) ;
#4088 = EDGE_CURVE ( 'NONE', #669, #776, #9384, .T. ) ;
#4089 = ORIENTED_EDGE ( 'NONE', *, *, #4217, .T. ) ;
#4090 = CARTESIAN_POINT ( 'NONE',  ( 1.128215178125001161, -4.940624999385482496, 1.954126010382870815 ) ) ;
#4091 = CARTESIAN_POINT ( 'NONE',  ( -11.36312591709337383, 0.8999999989075252449, 27.43301269999999548 ) ) ;
#4092 = FILL_AREA_STYLE ('',( #9587 ) ) ;
#4093 = LINE ( 'NONE', #3165, #4417 ) ;
#4094 = CARTESIAN_POINT ( 'NONE',  ( 27.00000000000000355, 4.800000000000000711, 0.000000000000000000 ) ) ;
#4095 = DIRECTION ( 'NONE',  ( 1.000000000000000000, 0.000000000000000000, 0.000000000000000000 ) ) ;
#4096 = CIRCLE ( 'NONE', #8106, 23.99999999999999645 ) ;
#4097 = ORIENTED_EDGE ( 'NONE', *, *, #3309, .F. ) ;
#4098 = SURFACE_STYLE_FILL_AREA ( #8861 ) ;
#4099 = CARTESIAN_POINT ( 'NONE',  ( 1.653273178848927064E-15, 0.2000000000000000111, -27.00000000000000355 ) ) ;
#4100 = ORIENTED_EDGE ( 'NONE', *, *, #5883, .T. ) ;
#4101 = ORIENTED_EDGE ( 'NONE', *, *, #4381, .F. ) ;
#4102 = CARTESIAN_POINT ( 'NONE',  ( 11.18376618407357093, 0.1500000000000000222, -27.00000000000000355 ) ) ;
#4103 = EDGE_CURVE ( 'NONE', #10097, #9021, #5294, .T. ) ;
#4104 = LINE ( 'NONE', #2727, #6614 ) ;
#4105 = CARTESIAN_POINT ( 'NONE',  ( 3.472565890032746960, 100.0000000000000284, -24.54662015932514052 ) ) ;
#4106 = B_SPLINE_SURFACE_WITH_KNOTS ( 'NONE', 3, 1, ( 
 ( #5900, #4182 ),
 ( #2711, #3390 ),
 ( #945, #9772 ),
 ( #6537, #304 ),
 ( #1814, #6581 ),
 ( #4138, #8258 ),
 ( #5006, #1088 ),
 ( #251, #7363 ),
 ( #5757, #5848 ),
 ( #1137, #7463 ),
 ( #5802, #9096 ),
 ( #8945, #1914 ),
 ( #5108, #2611 ),
 ( #3492, #9726 ),
 ( #6678, #4330 ),
 ( #7514, #8994 ),
 ( #8899, #9043 ),
 ( #8205, #1763 ),
 ( #3438, #6630 ) ),
 .UNSPECIFIED., .F., .F., .F.,
 ( 4, 1, 1, 1, 1, 1, 1, 1, 1, 1, 1, 1, 1, 1, 1, 1, 4 ),
 ( 2, 2 ),
 ( 0.000000000000000000, 0.06463354665699841406, 0.1274839167070160040, 0.1893660780973640267, 0.2502738481868047038, 0.3108090901939400408, 0.3728692346228669741, 0.4358265942208103261, 0.5002515515682643965, 0.5647461136436963125, 0.6273730017603231790, 0.6892793264321037672, 0.7497280364991398827, 0.8111249352628771003, 0.8723480300361200479, 0.9354359082354426480, 1.000000000000000000 ),
 ( 0.000000000000000000, 1.000000000000000000 ),
 .UNSPECIFIED. ) ;
#4107 = CARTESIAN_POINT ( 'NONE',  ( -1.595409442497313560E-16, -3.065624999385482496, -2.605501347177161087 ) ) ;
#4108 = CARTESIAN_POINT ( 'NONE',  ( -4.959819536546781389E-15, 1.999999997815050445, 27.00000000000000355 ) ) ;
#4110 = EDGE_CURVE ( 'NONE', #7728, #6767, #1048, .T. ) ;
#4109 = AXIS2_PLACEMENT_3D ( 'NONE', #5261, #5533, #1288 ) ;
#4111 = CARTESIAN_POINT ( 'NONE',  ( -22.51767453479306980, 99.50000000000000000, -9.764155749770198511 ) ) ;
#4112 = CARTESIAN_POINT ( 'NONE',  ( 5.047889085735837611, 100.0000000000000142, -24.22022158424849536 ) ) ;
#4113 = CARTESIAN_POINT ( 'NONE',  ( 1.249999999999999334, -4.593749998770965348, -2.165063509461096825 ) ) ;
#4114 = ORIENTED_EDGE ( 'NONE', *, *, #9672, .T. ) ;
#4115 = EDGE_CURVE ( 'NONE', #8517, #1976, #580, .T. ) ;
#4116 = DIRECTION ( 'NONE',  ( -0.000000000000000000, -1.000000000000000000, -0.000000000000000000 ) ) ;
#4117 = CARTESIAN_POINT ( 'NONE',  ( -15.45548338988150938, 99.49999999999997158, 16.93306818456458984 ) ) ;
#4119 = AXIS2_PLACEMENT_3D ( 'NONE', #2633, #3467, #4353 ) ;
#4118 = CARTESIAN_POINT ( 'NONE',  ( -21.79668695291220715, 99.50000000000000000, -11.08213026643738353 ) ) ;
#4120 = CARTESIAN_POINT ( 'NONE',  ( 2.256430356250000102, -3.065624999385482496, -2.763330213280484622E-16 ) ) ;
#4121 = ORIENTED_EDGE ( 'NONE', *, *, #6082, .F. ) ;
#4122 = CARTESIAN_POINT ( 'NONE',  ( 8.063732359723156051, 99.50000000000001421, 20.72384750152746236 ) ) ;
#4123 =( BOUNDED_CURVE ( )  B_SPLINE_CURVE ( 2, ( #5042, #8018, #2803, #9683, #5988, #5888, #3587, #2523, #1848 ),
 .UNSPECIFIED., .F., .F. ) 
 B_SPLINE_CURVE_WITH_KNOTS ( ( 3, 2, 2, 2, 3 ),
 ( 0.4375000000000000000, 0.4444444444444444198, 0.4583333333333333148, 0.4722222222222222099, 0.4791666666666666852 ),
 .UNSPECIFIED. ) 
 CURVE ( )  GEOMETRIC_REPRESENTATION_ITEM ( )  RATIONAL_B_SPLINE_CURVE ( ( 0.9330127018922194093, 0.9330127018922194093, 1.000000000000000000, 0.8660254037844387076, 1.000000000000000000, 0.8660254037844387076, 1.000000000000000000, 0.9330127018922190762, 0.9330127018922194093 ) ) 
 REPRESENTATION_ITEM ( '' )  );
#4124 = CARTESIAN_POINT ( 'NONE',  ( -3.486133158594716510E-16, -2.362499999999999378, -2.500000000000000000 ) ) ;
#4125 = CARTESIAN_POINT ( 'NONE',  ( -16.25072943800822500, 100.0000000000000568, 15.30228603765648820 ) ) ;
#4126 = CARTESIAN_POINT ( 'NONE',  ( -11.18376618407356737, 4.250000000000000888, -27.00000000000000355 ) ) ;
#4127 = ORIENTED_EDGE ( 'NONE', *, *, #4973, .F. ) ;
#4128 = CARTESIAN_POINT ( 'NONE',  ( 3.775125937424839151, 99.50000000000000000, -21.41825520325024712 ) ) ;
#4129 = CARTESIAN_POINT ( 'NONE',  ( 0.000000000000000000, 0.000000000000000000, 0.000000000000000000 ) ) ;
#4130 = CARTESIAN_POINT ( 'NONE',  ( 8.322475189980043098, 99.50000000000001421, 19.72675386960232657 ) ) ;
#4131 = EDGE_CURVE ( 'NONE', #26, #4746, #4096, .T. ) ;
#4132 = DIRECTION ( 'NONE',  ( 0.000000000000000000, -1.000000000000000000, 0.000000000000000000 ) ) ;
#4133 = CARTESIAN_POINT ( 'NONE',  ( -27.00000000000000355, 0.9499999978150502900, -11.18376618407357093 ) ) ;
#4134 = CARTESIAN_POINT ( 'NONE',  ( 11.18376618407357626, 3.050000000000000711, 27.00000000000000000 ) ) ;
#4135 = CLOSED_SHELL ( 'NONE', ( #6324, #7183, #5741, #8759, #1412, #1144, #2232, #3130, #10322, #2690, #2509, #9951, #1279, #6814, #5751, #4544, #8126, #6776, #9178, #7328, #1083, #194, #4517, #9581, #6704, #7343, #9828, #10040, #2602, #12, #746, #1678, #4854, #9757, #10300, #1389, #5977, #5354, #4933, #1221, #6884, #5949, #2091, #7940, #5327, #4534, #74, #2504, #142, #10110, #4808, #8055, #4865, #4076, #4478, #9245, #5502, #6523, #8070, #5858, #2592, #5790, #6773, #3660, #5928, #58, #4883, #10356, #5216, #6407, #7166, #8706, #683, #2627, #761, #8318, #8901, #4657, #1319, #9988, #1729, #3367, #1901, #389, #7935, #8514, #7040, #4712, #3222, #5241, #9484, #655, #7048, #10242, #491, #7932, #8104, #4861, #6620, #9016, #4580, #1148, #8192, #3456, #5016, #1599 ) ) ;
#4136 = CARTESIAN_POINT ( 'NONE',  ( -16.63177974700816009, 100.0000000000000000, 16.59747536361813403 ) ) ;
#4137 = CARTESIAN_POINT ( 'NONE',  ( -15.69015368034045643, 99.50000000000001421, 16.64011368054243434 ) ) ;
#4138 = CARTESIAN_POINT ( 'NONE',  ( -21.58460863908062066, 99.50000000000002842, -11.10356610083683648 ) ) ;
#4139 = COLOUR_RGB ( '',0.8941176470588234615, 0.8941176470588234615, 0.8941176470588234615 ) ;
#4140 = CARTESIAN_POINT ( 'NONE',  ( 1.128215178125001161, -3.590624999385482408, 1.954126010382870815 ) ) ;
#4141 = VERTEX_POINT ( 'NONE', #6914 ) ;
#4142 = CARTESIAN_POINT ( 'NONE',  ( 1.128215178125001161, -4.040624999385483029, 1.954126010382870815 ) ) ;
#4143 = CARTESIAN_POINT ( 'NONE',  ( -15.89341924297059094, 99.50000000000001421, 17.07725933521297890 ) ) ;
#4144 = CARTESIAN_POINT ( 'NONE',  ( 27.43301270000000258, 1.099999998907525089, -11.36312591709336139 ) ) ;
#4145 = ORIENTED_EDGE ( 'NONE', *, *, #9018, .T. ) ;
#4146 = EDGE_CURVE ( 'NONE', #2404, #9406, #483, .T. ) ;
#4147 = DIRECTION ( 'NONE',  ( -0.000000000000000000, -1.000000000000000000, -0.000000000000000000 ) ) ;
#4148 = CARTESIAN_POINT ( 'NONE',  ( 2.500000000000000000, -3.337499999999999467, -1.443375672974065438 ) ) ;
#4149 = DIRECTION ( 'NONE',  ( 0.000000000000000000, -1.000000000000000000, 0.000000000000000000 ) ) ;
#4150 = ORIENTED_EDGE ( 'NONE', *, *, #5314, .F. ) ;
#4151 = ORIENTED_EDGE ( 'NONE', *, *, #5083, .T. ) ;
#4152 = CARTESIAN_POINT ( 'NONE',  ( 27.43301270000000258, 4.299999998907525267, -11.36312591709336139 ) ) ;
#4153 = CARTESIAN_POINT ( 'NONE',  ( 3.606694021351891877, 100.0000000000000000, -24.61315535935035115 ) ) ;
#4154 = DIRECTION ( 'NONE',  ( 0.000000000000000000, 0.000000000000000000, 1.000000000000000000 ) ) ;
#4155 = CIRCLE ( 'NONE', #8833, 25.15000000000000213 ) ;
#4156 = CARTESIAN_POINT ( 'NONE',  ( 1.128215178125001161, -4.603124999385482141, 1.954126010382870815 ) ) ;
#4157 = CARTESIAN_POINT ( 'NONE',  ( -22.67341330918043951, 99.50000000000000000, -10.57563951594260665 ) ) ;
#4158 = CARTESIAN_POINT ( 'NONE',  ( -16.62994343074595349, 99.99999999999998579, 15.18287566599475191 ) ) ;
#4159 = DIRECTION ( 'NONE',  ( -0.000000000000000000, 1.000000000000000000, -0.000000000000000000 ) ) ;
#4160 = CARTESIAN_POINT ( 'NONE',  ( -1.250000000000000222, -4.968749998770965348, -2.165063509461096825 ) ) ;
#4161 = ORIENTED_EDGE ( 'NONE', *, *, #9147, .F. ) ;
#4162 = FACE_OUTER_BOUND ( 'NONE', #10001, .T. ) ;
#4163 = CARTESIAN_POINT ( 'NONE',  ( 3.204253864046738176, 99.99999999999997158, -22.06071064728738662 ) ) ;
#4164 = CARTESIAN_POINT ( 'NONE',  ( -21.51485068221570174, 99.50000000000000000, -11.09552232883975087 ) ) ;
#4165 = CARTESIAN_POINT ( 'NONE',  ( -1.595409442497313560E-16, -3.403124999385483296, -2.605501347177161087 ) ) ;
#4166 = EDGE_CURVE ( 'NONE', #2986, #405, #7646, .T. ) ;
#4167 = ORIENTED_EDGE ( 'NONE', *, *, #3987, .T. ) ;
#4168 = EDGE_CURVE ( 'NONE', #653, #8788, #10174, .T. ) ;
#4169 = ORIENTED_EDGE ( 'NONE', *, *, #9725, .T. ) ;
#4170 = DIRECTION ( 'NONE',  ( -0.000000000000000000, 1.000000000000000000, -0.000000000000000000 ) ) ;
#4171 = LINE ( 'NONE', #5744, #3167 ) ;
#4172 = DIRECTION ( 'NONE',  ( 0.08715574274765837404, -0.9961946980917455452, 0.000000000000000000 ) ) ;
#4173 = DIRECTION ( 'NONE',  ( 0.000000000000000000, 0.000000000000000000, -1.000000000000000000 ) ) ;
#4174 = CARTESIAN_POINT ( 'NONE',  ( 3.504547665631520648, 99.49999999999997158, -23.10026541809159184 ) ) ;
#4175 = CARTESIAN_POINT ( 'NONE',  ( -20.72805389903318130, 100.0000000000000000, -9.848585782927868237 ) ) ;
#4176 = CARTESIAN_POINT ( 'NONE',  ( 9.873655262861264603, 99.50000000000000000, 20.34710108723753308 ) ) ;
#4177 = CARTESIAN_POINT ( 'NONE',  ( 19.09188309203678102, 3.699999997815051067, 19.09188309203678813 ) ) ;
#4178 =( BOUNDED_CURVE ( )  B_SPLINE_CURVE ( 2, ( #768, #2284, #2968, #4637, #8563, #5484, #5777, #1787, #8872 ),
 .UNSPECIFIED., .F., .F. ) 
 B_SPLINE_CURVE_WITH_KNOTS ( ( 3, 2, 2, 2, 3 ),
 ( 0.3125000000000000000, 0.3194444444444444198, 0.3333333333333333148, 0.3472222222222222099, 0.3541666666666666852 ),
 .UNSPECIFIED. ) 
 CURVE ( )  GEOMETRIC_REPRESENTATION_ITEM ( )  RATIONAL_B_SPLINE_CURVE ( ( 0.9330127018922194093, 0.9330127018922194093, 1.000000000000000000, 0.8660254037844387076, 1.000000000000000000, 0.8660254037844387076, 1.000000000000000000, 0.9330127018922190762, 0.9330127018922194093 ) ) 
 REPRESENTATION_ITEM ( '' )  );
#4179 = CARTESIAN_POINT ( 'NONE',  ( -20.79740905086423552, 99.50000000000001421, -11.06234285579171051 ) ) ;
#4180 = FACE_OUTER_BOUND ( 'NONE', #9430, .T. ) ;
#4181 = CARTESIAN_POINT ( 'NONE',  ( 0.000000000000000000, 0.000000000000000000, -2.500000000000000000 ) ) ;
#4182 = CARTESIAN_POINT ( 'NONE',  ( -21.30928386698190025, 100.0000000000000000, -11.02857376369709996 ) ) ;
#4183 = AXIS2_PLACEMENT_3D ( 'NONE', #4430, #4378, #4594 ) ;
#4184 = ORIENTED_EDGE ( 'NONE', *, *, #3276, .F. ) ;
#4185 = CARTESIAN_POINT ( 'NONE',  ( -2.256430356249999214, -3.703124999385482674, 1.302750673588581876 ) ) ;
#4186 = DIRECTION ( 'NONE',  ( 1.000000000000000000, 0.000000000000000000, 0.000000000000000000 ) ) ;
#4187 = CARTESIAN_POINT ( 'NONE',  ( -15.42740294075255925, 99.50000000000000000, 14.91894146668702348 ) ) ;
#4188 = CARTESIAN_POINT ( 'NONE',  ( -2.256430356250000102, -0.7406249993854829849, -1.302750673588580321 ) ) ;
#4189 = CARTESIAN_POINT ( 'NONE',  ( -27.00000000000001421, 2.850000000000000089, 11.18376618407356382 ) ) ;
#4190 = CARTESIAN_POINT ( 'NONE',  ( 19.39806930854668110, 0.4499999989075251783, -19.39806930854668110 ) ) ;
#4191 = DIRECTION ( 'NONE',  ( -0.000000000000000000, -1.000000000000000000, -0.000000000000000000 ) ) ;
#4192 = CARTESIAN_POINT ( 'NONE',  ( 0.000000000000000000, 97.00000000000000000, 0.000000000000000000 ) ) ;
#4193 = CARTESIAN_POINT ( 'NONE',  ( -20.96129225301843135, 99.50000000000001421, -10.68089388303413934 ) ) ;
#4194 = EDGE_LOOP ( 'NONE', ( #4343, #3095, #4575, #9751 ) ) ;
#4195 = CARTESIAN_POINT ( 'NONE',  ( -21.69499712064247277, 99.49999999999998579, -9.295461156691713356 ) ) ;
#4196 = CARTESIAN_POINT ( 'NONE',  ( 1.250000000000001110, -1.593749998770965792, 2.165063509461096380 ) ) ;
#4197 = CARTESIAN_POINT ( 'NONE',  ( 19.39806930854668110, 0.3499999989075252005, -19.39806930854668110 ) ) ;
#4198 = EDGE_CURVE ( 'NONE', #10197, #8050, #9656, .T. ) ;
#4199 = CARTESIAN_POINT ( 'NONE',  ( 4.405197143102897783, 99.99999999999995737, -21.72932741277565682 ) ) ;
#4200 = LINE ( 'NONE', #3767, #547 ) ;
#4201 = CARTESIAN_POINT ( 'NONE',  ( -16.67860655220511035, 99.99999999999998579, 15.23428378554110374 ) ) ;
#4202 = CARTESIAN_POINT ( 'NONE',  ( 4.295198626299898237, 100.0000000000000142, -24.68029520312135361 ) ) ;
#4203 = ORIENTED_EDGE ( 'NONE', *, *, #2251, .F. ) ;
#4204 = CARTESIAN_POINT ( 'NONE',  ( -1.595409442497313560E-16, -0.3656249993854829294, -2.605501347177161087 ) ) ;
#4205 = ORIENTED_EDGE ( 'NONE', *, *, #4220, .T. ) ;
#4206 = VECTOR ( 'NONE', #1842, 1000.000000000000000 ) ;
#4207 = CARTESIAN_POINT ( 'NONE',  ( 3.861186820804014097, 100.0000000000000426, -21.07288982789904708 ) ) ;
#4208 = CARTESIAN_POINT ( 'NONE',  ( 3.231466532446834350, 99.99999999999994316, -21.81145066552309686 ) ) ;
#4209 = EDGE_CURVE ( 'NONE', #4294, #1061, #591, .T. ) ;
#4210 = CARTESIAN_POINT ( 'NONE',  ( 9.806436918512124734, 99.49999999999998579, 20.18080982695387604 ) ) ;
#4211 = LINE ( 'NONE', #8287, #4206 ) ;
#4212 = VERTEX_POINT ( 'NONE', #3010 ) ;
#4213 = AXIS2_PLACEMENT_3D ( 'NONE', #6703, #8334, #4410 ) ;
#4214 = CARTESIAN_POINT ( 'NONE',  ( 2.500000000000000444, -1.612499999999999822, 1.443375672974063439 ) ) ;
#4215 = PRODUCT_DEFINITION ( 'UNKNOWN', '', #6632, #2461 ) ;
#4216 = FACE_OUTER_BOUND ( 'NONE', #6879, .T. ) ;
#4217 = EDGE_CURVE ( 'NONE', #7000, #3016, #4249, .T. ) ;
#4218 = CARTESIAN_POINT ( 'NONE',  ( -9.703070624755296135E-15, -3.881249998770965881, 2.500000000000000444 ) ) ;
#4219 =( GEOMETRIC_REPRESENTATION_CONTEXT ( 3 ) GLOBAL_UNCERTAINTY_ASSIGNED_CONTEXT ( ( #7799 ) ) GLOBAL_UNIT_ASSIGNED_CONTEXT ( ( #6798, #3616, #1099 ) ) REPRESENTATION_CONTEXT ( 'NONE', 'WORKASPACE' ) );
#4220 = EDGE_CURVE ( 'NONE', #6813, #872, #643, .T. ) ;
#4221 = CARTESIAN_POINT ( 'NONE',  ( 0.000000000000000000, 97.50000000000000000, 0.000000000000000000 ) ) ;
#4222 = CARTESIAN_POINT ( 'NONE',  ( 3.171774962637509798, 99.50000000000000000, -24.28498992023182268 ) ) ;
#4223 = CARTESIAN_POINT ( 'NONE',  ( 8.223467485077383898, 99.99999999999992895, 19.78581333328655134 ) ) ;
#4224 = EDGE_CURVE ( 'NONE', #3171, #957, #11, .T. ) ;
#4225 = ORIENTED_EDGE ( 'NONE', *, *, #2364, .T. ) ;
#4226 = CARTESIAN_POINT ( 'NONE',  ( 2.964854786877021642, 99.50000000000000000, -22.43901021186594846 ) ) ;
#4227 = CARTESIAN_POINT ( 'NONE',  ( -19.09188309203678457, 3.299999997815050712, -19.09188309203678813 ) ) ;
#4228 = LINE ( 'NONE', #2708, #8539 ) ;
#4229 = CARTESIAN_POINT ( 'NONE',  ( -20.97771390646102319, 100.0000000000000284, -10.03345247102482674 ) ) ;
#4230 = DIRECTION ( 'NONE',  ( 0.000000000000000000, -0.000000000000000000, -1.000000000000000000 ) ) ;
#4231 = CARTESIAN_POINT ( 'NONE',  ( 9.342627931057743140, 99.50000000000000000, 21.59831790269294771 ) ) ;
#4232 = CARTESIAN_POINT ( 'NONE',  ( 3.106448761625311139, 99.99999999999998579, -21.38062202216113761 ) ) ;
#4233 = DIRECTION ( 'NONE',  ( 0.000000000000000000, 1.000000000000000000, 0.000000000000000000 ) ) ;
#4234 = ORIENTED_EDGE ( 'NONE', *, *, #9051, .F. ) ;
#4235 = CARTESIAN_POINT ( 'NONE',  ( 2.256430356249999658, -3.478124999385482585, -1.302750673588581432 ) ) ;
#4236 = SURFACE_SIDE_STYLE ('',( #5854 ) ) ;
#4237 = CARTESIAN_POINT ( 'NONE',  ( -14.76042637754942177, 99.99999999999998579, 16.05242888258284140 ) ) ;
#4238 = CARTESIAN_POINT ( 'NONE',  ( -2.256430356250000102, -0.2531249993854829405, 0.000000000000000000 ) ) ;
#4239 = CARTESIAN_POINT ( 'NONE',  ( 19.39806930854668110, 1.949999998907525178, -19.39806930854668110 ) ) ;
#4240 = CARTESIAN_POINT ( 'NONE',  ( 3.306546357697854128E-15, 0.000000000000000000, 27.00000000000000355 ) ) ;
#4241 = CYLINDRICAL_SURFACE ( 'NONE', #603, 2.500000000000000000 ) ;
#4242 = CARTESIAN_POINT ( 'NONE',  ( 7.486453019397995234, 99.50000000000000000, 23.81666162955709964 ) ) ;
#4243 = CARTESIAN_POINT ( 'NONE',  ( 7.809833820264425519, 99.99999999999995737, 20.29999375863051370 ) ) ;
#4244 = VERTEX_POINT ( 'NONE', #7278 ) ;
#4245 = CARTESIAN_POINT ( 'NONE',  ( 7.913184448816831029, 99.50000000000000000, 20.09878816755126252 ) ) ;
#4246 = CARTESIAN_POINT ( 'NONE',  ( 4.295198626299898237, 100.0000000000000142, -24.68029520312135361 ) ) ;
#4247 = CARTESIAN_POINT ( 'NONE',  ( 3.306546357697854128E-15, 100.0000000000000000, 27.00000000000000355 ) ) ;
#4248 = CARTESIAN_POINT ( 'NONE',  ( -16.12311789350856017, 99.99999999999995737, 14.86696503675854686 ) ) ;
#4249 = CIRCLE ( 'NONE', #5247, 20.00000000000000000 ) ;
#4250 = DIRECTION ( 'NONE',  ( 0.000000000000000000, 0.000000000000000000, -1.000000000000000000 ) ) ;
#4251 = CARTESIAN_POINT ( 'NONE',  ( -22.57971655928959365, 99.50000000000000000, -10.84768434062017839 ) ) ;
#4252 = CARTESIAN_POINT ( 'NONE',  ( -21.73488407773357167, 100.0000000000000000, -9.647150398373231184 ) ) ;
#4253 = ORIENTED_EDGE ( 'NONE', *, *, #8937, .F. ) ;
#4254 = EDGE_CURVE ( 'NONE', #5320, #7728, #7662, .T. ) ;
#4255 = CARTESIAN_POINT ( 'NONE',  ( 1.250000000000001110, -4.743749998770965703, 2.165063509461096380 ) ) ;
#4256 = ORIENTED_EDGE ( 'NONE', *, *, #2997, .T. ) ;
#4257 = CARTESIAN_POINT ( 'NONE',  ( -22.22752541189434794, 99.99999999999994316, -11.26717589342885084 ) ) ;
#4258 = CARTESIAN_POINT ( 'NONE',  ( 3.254133136943549776, 99.50000000000000000, -21.76036676155726823 ) ) ;
#4259 = VECTOR ( 'NONE', #8404, 1000.000000000000227 ) ;
#4260 = CARTESIAN_POINT ( 'NONE',  ( 3.275092494823534928, 99.50000000000000000, -23.54688978826290580 ) ) ;
#4261 = CARTESIAN_POINT ( 'NONE',  ( -27.00000000000000355, 3.349999997815050534, -11.18376618407357270 ) ) ;
#4262 = CIRCLE ( 'NONE', #2441, 1.324999999999999734 ) ;
#4263 = ADVANCED_FACE ( 'NONE', ( #117 ), #5669, .T. ) ;
#4264 = CYLINDRICAL_SURFACE ( 'NONE', #615, 23.99999999999999645 ) ;
#4265 = DIRECTION ( 'NONE',  ( -0.000000000000000000, -1.000000000000000000, -0.000000000000000000 ) ) ;
#4266 = CARTESIAN_POINT ( 'NONE',  ( -21.72555844818415594, 100.0000000000000142, -11.09629251537910655 ) ) ;
#4267 = CIRCLE ( 'NONE', #1704, 24.00000000000000355 ) ;
#4268 = CARTESIAN_POINT ( 'NONE',  ( 4.054941747578200584, 99.49999999999998579, -24.36678493958047298 ) ) ;
#4269 = ORIENTED_EDGE ( 'NONE', *, *, #2251, .T. ) ;
#4270 = CARTESIAN_POINT ( 'NONE',  ( 9.877377282685029372E-16, -0.7312499987709657479, 2.500000000000000000 ) ) ;
#4271 = CARTESIAN_POINT ( 'NONE',  ( -27.43301270000000258, 4.699999998907525622, -11.36312591709336317 ) ) ;
#4272 = FACE_OUTER_BOUND ( 'NONE', #6236, .T. ) ;
#4273 = CARTESIAN_POINT ( 'NONE',  ( 3.573144549190039321, 99.99999999999995737, -23.04580706645134214 ) ) ;
#4274 = CARTESIAN_POINT ( 'NONE',  ( 8.322475189980043098, 99.99999999999995737, 19.72675386960232657 ) ) ;
#4275 = ORIENTED_EDGE ( 'NONE', *, *, #2074, .F. ) ;
#4276 = CARTESIAN_POINT ( 'NONE',  ( -20.72805389903318130, 100.0000000000000000, -9.848585782927868237 ) ) ;
#4277 = CARTESIAN_POINT ( 'NONE',  ( 11.18376618407356915, 3.149999997815050801, -27.00000000000000355 ) ) ;
#4278 = CARTESIAN_POINT ( 'NONE',  ( 0.000000000000000000, 72.50000000000001421, 0.000000000000000000 ) ) ;
#4279 = DIRECTION ( 'NONE',  ( 1.000000000000000000, 0.000000000000000000, 4.336808689942017736E-16 ) ) ;
#4280 = DIRECTION ( 'NONE',  ( 0.2907756355032780071, 0.000000000000000000, 0.9567912676219745283 ) ) ;
#4281 = CARTESIAN_POINT ( 'NONE',  ( -22.50000000000000355, 0.000000000000000000, 1.622657008870243228E-16 ) ) ;
#4282 = ORIENTED_EDGE ( 'NONE', *, *, #1843, .T. ) ;
#4283 = AXIS2_PLACEMENT_3D ( 'NONE', #5865, #912, #9741 ) ;
#4284 = CARTESIAN_POINT ( 'NONE',  ( 1.128215178125001161, -4.490624999385482319, 1.954126010382870815 ) ) ;
#4285 = CARTESIAN_POINT ( 'NONE',  ( -14.75894607058735630, 100.0000000000000142, 15.77473972644577849 ) ) ;
#4286 = CARTESIAN_POINT ( 'NONE',  ( 0.000000000000000000, 73.81339255365637086, 0.000000000000000000 ) ) ;
#4287 = CARTESIAN_POINT ( 'NONE',  ( -11.36312591709337383, 3.199999998907524734, 27.43301269999999548 ) ) ;
#4288 = CARTESIAN_POINT ( 'NONE',  ( 0.000000000000000000, 0.000000000000000000, 1.622657008870242981E-16 ) ) ;
#4289 = VECTOR ( 'NONE', #4489, 1000.000000000000000 ) ;
#4290 = EDGE_CURVE ( 'NONE', #2960, #6092, #8044, .T. ) ;
#4291 = CARTESIAN_POINT ( 'NONE',  ( 0.000000000000000000, 100.0000000000000000, 0.000000000000000000 ) ) ;
#4292 = VECTOR ( 'NONE', #7248, 1000.000000000000000 ) ;
#4293 = CARTESIAN_POINT ( 'NONE',  ( 4.457146071884139360, 100.0000000000000142, -24.28472590373185724 ) ) ;
#4294 = VERTEX_POINT ( 'NONE', #9639 ) ;
#4295 = CARTESIAN_POINT ( 'NONE',  ( -20.89052720883767122, 99.99999999999994316, -9.602653601535816819 ) ) ;
#4296 = CARTESIAN_POINT ( 'NONE',  ( -5.039362679103552881E-15, 4.849999998907525089, 27.43301270000000258 ) ) ;
#4297 = FACE_OUTER_BOUND ( 'NONE', #5570, .T. ) ;
#4298 = LINE ( 'NONE', #1057, #2257 ) ;
#4299 = CARTESIAN_POINT ( 'NONE',  ( -16.42071764973191250, 100.0000000000000142, 16.76105279315999042 ) ) ;
#4300 = CARTESIAN_POINT ( 'NONE',  ( 9.389534246205572643, 99.99999999999994316, 21.46805835725047729 ) ) ;
#4301 = DIRECTION ( 'NONE',  ( 0.000000000000000000, -1.000000000000000000, 0.000000000000000000 ) ) ;
#4302 = VERTEX_POINT ( 'NONE', #6498 ) ;
#4303 = CARTESIAN_POINT ( 'NONE',  ( -15.83671465916681242, 99.50000000000000000, 16.65403364262263608 ) ) ;
#4304 = CARTESIAN_POINT ( 'NONE',  ( 4.786228327491941173E-16, -1.040624999385482585, 2.605501347177161087 ) ) ;
#4305 = EDGE_LOOP ( 'NONE', ( #3992, #7378, #6064, #4487 ) ) ;
#4306 = AXIS2_PLACEMENT_3D ( 'NONE', #9783, #3399, #4971 ) ;
#4307 = DIRECTION ( 'NONE',  ( -0.000000000000000000, 1.000000000000000000, -0.000000000000000000 ) ) ;
#4308 = CARTESIAN_POINT ( 'NONE',  ( 3.317038232150706367, 99.49999999999998579, -21.66195598387956878 ) ) ;
#4309 = CARTESIAN_POINT ( 'NONE',  ( 3.282077632710153292, 99.50000000000000000, -23.74569985055724786 ) ) ;
#4310 = DIRECTION ( 'NONE',  ( -0.000000000000000000, -1.000000000000000000, -0.000000000000000000 ) ) ;
#4311 = AXIS2_PLACEMENT_3D ( 'NONE', #9712, #7397, #1709 ) ;
#4312 = ORIENTED_EDGE ( 'NONE', *, *, #5630, .F. ) ;
#4313 = CARTESIAN_POINT ( 'NONE',  ( -16.52157078939288937, 99.99999999999994316, 16.20087177393598665 ) ) ;
#4314 = DIRECTION ( 'NONE',  ( 0.000000000000000000, 1.000000000000000000, -0.000000000000000000 ) ) ;
#4315 = DIRECTION ( 'NONE',  ( 0.9853569121566161382, 0.000000000000000000, 0.1705044153832351028 ) ) ;
#4316 = CARTESIAN_POINT ( 'NONE',  ( 0.000000000000000000, 97.00000000000000000, 0.000000000000000000 ) ) ;
#4317 = ORIENTED_EDGE ( 'NONE', *, *, #8937, .T. ) ;
#4318 = DIRECTION ( 'NONE',  ( 1.000000000000000000, 0.000000000000000000, 0.000000000000000000 ) ) ;
#4319 = CARTESIAN_POINT ( 'NONE',  ( -27.43301270000000258, 2.349999998907525534, -3.359575119402369376E-15 ) ) ;
#4320 = CARTESIAN_POINT ( 'NONE',  ( 3.079986699855593473E-15, 0.000000000000000000, 25.15000000000000213 ) ) ;
#4321 = ADVANCED_FACE ( 'NONE', ( #949 ), #7127, .T. ) ;
#4322 = CARTESIAN_POINT ( 'NONE',  ( 3.891852272358404807, 99.50000000000001421, -22.89765557720719968 ) ) ;
#4323 = CARTESIAN_POINT ( 'NONE',  ( 4.187832255138415505, 99.99999999999998579, -21.50835573230103037 ) ) ;
#4324 = ORIENTED_EDGE ( 'NONE', *, *, #780, .T. ) ;
#4325 = CARTESIAN_POINT ( 'NONE',  ( 3.222930479149370253, 99.99999999999998579, -22.15251218086615381 ) ) ;
#4326 = CARTESIAN_POINT ( 'NONE',  ( -4.959819536546781389E-15, 4.399999997815050357, 27.00000000000000355 ) ) ;
#4327 = DIRECTION ( 'NONE',  ( -0.9198211419112228837, 0.000000000000000000, 0.3923379498508065000 ) ) ;
#4328 = CARTESIAN_POINT ( 'NONE',  ( -21.87421819196487505, 100.0000000000000000, -9.684578881761979119 ) ) ;
#4329 = CARTESIAN_POINT ( 'NONE',  ( 3.434779879277784609, 100.0000000000000142, -23.17575050830969374 ) ) ;
#4330 = CARTESIAN_POINT ( 'NONE',  ( -22.16320288552370243, 100.0000000000000142, -10.86869938533413915 ) ) ;
#4331 = CARTESIAN_POINT ( 'NONE',  ( -23.82500000000000284, 0.000000000000000000, 0.000000000000000000 ) ) ;
#4332 = CARTESIAN_POINT ( 'NONE',  ( -0.6698729810778054627, -4.801346188203300613, 2.500000000000000000 ) ) ;
#4333 = ORIENTED_EDGE ( 'NONE', *, *, #5586, .F. ) ;
#4334 = CARTESIAN_POINT ( 'NONE',  ( 5.302876193624534821E-16, -2.587499999999999911, 2.886751345948128655 ) ) ;
#4335 = APPLICATION_PROTOCOL_DEFINITION ( 'draft international standard', 'automotive_design', 1998, #8548 ) ;
#4336 = CARTESIAN_POINT ( 'NONE',  ( -15.17782247516205274, 99.49999999999998579, 15.06300032623928686 ) ) ;
#4337 = CARTESIAN_POINT ( 'NONE',  ( 3.044406660298407452, 99.50000000000000000, -23.15442635585071685 ) ) ;
#4338 = CARTESIAN_POINT ( 'NONE',  ( 11.36312591709336139, 3.599999998907525089, -27.43301270000000258 ) ) ;
#4339 = CARTESIAN_POINT ( 'NONE',  ( -20.52076770522338833, 100.0000000000000000, -10.69798695537560462 ) ) ;
#4340 = CARTESIAN_POINT ( 'NONE',  ( -21.30928386698190025, 99.50000000000000000, -11.02857376369709996 ) ) ;
#4341 = CARTESIAN_POINT ( 'NONE',  ( 4.259295290443009918, 100.0000000000000284, -24.34414156132068996 ) ) ;
#4342 = CARTESIAN_POINT ( 'NONE',  ( -19.09188309203678457, 4.099999997815050534, -19.09188309203678813 ) ) ;
#4343 = ORIENTED_EDGE ( 'NONE', *, *, #8719, .F. ) ;
#4344 = CARTESIAN_POINT ( 'NONE',  ( 0.000000000000000000, 75.00000000000001421, 0.000000000000000000 ) ) ;
#4345 = CARTESIAN_POINT ( 'NONE',  ( -2.500000000000000000, -4.087500000000000355, -1.443375672974064106 ) ) ;
#4346 = ADVANCED_FACE ( 'NONE', ( #7969 ), #8904, .T. ) ;
#4347 = CARTESIAN_POINT ( 'NONE',  ( 4.786228327491941173E-16, -0.4781249993854829183, 2.605501347177161087 ) ) ;
#4348 = LINE ( 'NONE', #1055, #356 ) ;
#4349 = EDGE_CURVE ( 'NONE', #827, #7488, #4093, .T. ) ;
#4350 = CARTESIAN_POINT ( 'NONE',  ( 4.486604876299897349, 100.0000000000000000, -21.85617661337775885 ) ) ;
#4351 = DIRECTION ( 'NONE',  ( 0.000000000000000000, 0.000000000000000000, 1.000000000000000000 ) ) ;
#4352=STYLED_ITEM('',(#10394),#6259);
#4353 = DIRECTION ( 'NONE',  ( 0.000000000000000000, 0.000000000000000000, -1.000000000000000000 ) ) ;
#4354 = ORIENTED_EDGE ( 'NONE', *, *, #5881, .T. ) ;
#4355 = CARTESIAN_POINT ( 'NONE',  ( 0.000000000000000000, 100.0000000000000000, 0.000000000000000000 ) ) ;
#4356 = CARTESIAN_POINT ( 'NONE',  ( -2.256430356249999214, -0.6656249993854828073, 1.302750673588581876 ) ) ;
#4357 = ORIENTED_EDGE ( 'NONE', *, *, #7145, .T. ) ;
#4358 = CARTESIAN_POINT ( 'NONE',  ( -22.28738277804067636, 99.49999999999997158, -10.06255608345902886 ) ) ;
#4359 = CARTESIAN_POINT ( 'NONE',  ( 9.820792995160308791, 99.50000000000000000, 20.21220011423140761 ) ) ;
#4360 = LINE ( 'NONE', #496, #8090 ) ;
#4361 = CARTESIAN_POINT ( 'NONE',  ( 1.653273178848927064E-15, 3.199999997815050623, -27.00000000000000355 ) ) ;
#4362 = VECTOR ( 'NONE', #8977, 1000.000000000000114 ) ;
#4363 = CARTESIAN_POINT ( 'NONE',  ( -16.52319226728147328, 99.99999999999994316, 15.63609008536095324 ) ) ;
#4364 = CARTESIAN_POINT ( 'NONE',  ( 4.118246196500586542, 99.49999999999998579, -21.10643963665684453 ) ) ;
#4365 = ORIENTED_EDGE ( 'NONE', *, *, #2818, .T. ) ;
#4366 = CARTESIAN_POINT ( 'NONE',  ( 1.249999999999999334, -3.693749998770965437, -2.165063509461096825 ) ) ;
#4367 = CARTESIAN_POINT ( 'NONE',  ( 9.563602730896748838, 100.0000000000000142, 20.87184380654744587 ) ) ;
#4368 = ORIENTED_EDGE ( 'NONE', *, *, #6527, .T. ) ;
#4369 = DIRECTION ( 'NONE',  ( 0.000000000000000000, -0.000000000000000000, -1.000000000000000000 ) ) ;
#4370 = CARTESIAN_POINT ( 'NONE',  ( 11.36312591709336139, 5.299999998907526155, -27.43301270000000258 ) ) ;
#4371 = CARTESIAN_POINT ( 'NONE',  ( -2.500000000000000000, -2.231249998770965970, -1.443375672974064106 ) ) ;
#4372 = VECTOR ( 'NONE', #3074, 1000.000000000000000 ) ;
#4373 = CARTESIAN_POINT ( 'NONE',  ( -18.01369080470046313, 100.0000000000000000, 17.15556831233607937 ) ) ;
#4374 = CARTESIAN_POINT ( 'NONE',  ( 4.154273145530666511, 99.50000000000000000, -22.82723029927519676 ) ) ;
#4375 = EDGE_LOOP ( 'NONE', ( #6784, #2279, #9380, #2862 ) ) ;
#4376 = CARTESIAN_POINT ( 'NONE',  ( 3.212364564527730337, 99.50000000000000000, -22.10366694310577884 ) ) ;
#4377 = CARTESIAN_POINT ( 'NONE',  ( -11.18376618407356560, 4.049999997815050712, -27.00000000000000355 ) ) ;
#4378 = DIRECTION ( 'NONE',  ( 0.000000000000000000, 1.000000000000000000, 0.000000000000000000 ) ) ;
#4379 = FACE_OUTER_BOUND ( 'NONE', #1630, .T. ) ;
#4380 = AXIS2_PLACEMENT_3D ( 'NONE', #8079, #908, #7526 ) ;
#4381 = EDGE_CURVE ( 'NONE', #1163, #2926, #2474, .T. ) ;
#4382 = ORIENTED_EDGE ( 'NONE', *, *, #8558, .T. ) ;
#4383 = CARTESIAN_POINT ( 'NONE',  ( 4.901590909071964042, 99.50000000000000000, -23.62641080846013608 ) ) ;
#4384 = CARTESIAN_POINT ( 'NONE',  ( -11.36312591709337561, 1.699999998907525178, 27.43301269999999548 ) ) ;
#4385 = ORIENTED_EDGE ( 'NONE', *, *, #3721, .T. ) ;
#4386 = CARTESIAN_POINT ( 'NONE',  ( 1.250000000000001110, -1.649999999999999689, 2.165063509461096380 ) ) ;
#4387 =( BOUNDED_CURVE ( )  B_SPLINE_CURVE ( 2, ( #3223, #6410, #915, #8767, #4007, #7192, #9696, #5680, #2974 ),
 .UNSPECIFIED., .F., .F. ) 
 B_SPLINE_CURVE_WITH_KNOTS ( ( 3, 2, 2, 2, 3 ),
 ( 0.03571428571428571230, 0.05357142857142856845, 0.07142857142857142461, 0.08928571428571428770, 0.1071428571428571369 ),
 .UNSPECIFIED. ) 
 CURVE ( )  GEOMETRIC_REPRESENTATION_ITEM ( )  RATIONAL_B_SPLINE_CURVE ( ( 1.000000000000000000, 0.9238795325112867385, 1.000000000000000000, 0.9238795325112867385, 1.000000000000000000, 0.9238795325112867385, 1.000000000000000000, 0.9238795325112867385, 1.000000000000000000 ) ) 
 REPRESENTATION_ITEM ( '' )  );
#4388 = SHAPE_DEFINITION_REPRESENTATION ( #9536, #2324 ) ;
#4389 = CARTESIAN_POINT ( 'NONE',  ( -14.75894607058735630, 99.50000000000002842, 15.77473972644577849 ) ) ;
#4390 = CARTESIAN_POINT ( 'NONE',  ( 2.256430356250000546, -0.5156249993854828961, 1.302750673588579877 ) ) ;
#4391 = CARTESIAN_POINT ( 'NONE',  ( -11.36312591709335962, 1.299999998907525267, -27.43301270000000258 ) ) ;
#4392 = CARTESIAN_POINT ( 'NONE',  ( -1.249999999999998224, -0.8249999999999998446, 2.165063509461097713 ) ) ;
#4393 = COLOUR_RGB ( '',0.8941176470588234615, 0.8941176470588234615, 0.8941176470588234615 ) ;
#4394 = CARTESIAN_POINT ( 'NONE',  ( -15.76250887235353737, 99.99999999999998579, 16.65066592061022277 ) ) ;
#4395 = DIRECTION ( 'NONE',  ( 0.000000000000000000, 0.000000000000000000, -1.000000000000000000 ) ) ;
#4396 = CARTESIAN_POINT ( 'NONE',  ( 7.826802610544922878, 100.0000000000000000, 21.21129867192371421 ) ) ;
#4397 = EDGE_CURVE ( 'NONE', #7345, #4075, #9588, .T. ) ;
#4398 = CARTESIAN_POINT ( 'NONE',  ( 4.143207896384923039, 99.99999999999998579, -24.36264353342416911 ) ) ;
#4399 = CARTESIAN_POINT ( 'NONE',  ( -21.03505001771060634, 99.50000000000000000, -9.476849197711761263 ) ) ;
#4400 = CARTESIAN_POINT ( 'NONE',  ( 21.82251602564102910, 99.50000000000000000, -0.5181290064102563875 ) ) ;
#4401 = ORIENTED_EDGE ( 'NONE', *, *, #6874, .T. ) ;
#4402 = CARTESIAN_POINT ( 'NONE',  ( -3.486133158594716510E-16, -1.406249998770965570, -2.500000000000000000 ) ) ;
#4403 = CARTESIAN_POINT ( 'NONE',  ( -27.43301270000000969, 0.6999999989075252893, 11.36312591709335429 ) ) ;
#4404 = B_SPLINE_CURVE_WITH_KNOTS ( 'NONE', 3,
 ( #8206, #5058, #72, #7515, #355, #1089, #4232, #8995, #7464, #9874, #5803, #5162, #1139, #2482, #3546 ),
 .UNSPECIFIED., .F., .F.,
 ( 4, 1, 1, 1, 1, 1, 1, 1, 1, 1, 1, 1, 4 ),
 ( 0.000000000000000000, 0.08963690308348271074, 0.1775767702671464110, 0.2649576542713044658, 0.3533131777157214604, 0.4402865524342069459, 0.5245518675747646853, 0.6066224975438009315, 0.6889424263984335051, 0.7698335385027974542, 0.8475882324521423206, 0.9236428641877653112, 1.000000000000000000 ),
 .UNSPECIFIED. ) ;
#4405 = EDGE_CURVE ( 'NONE', #6757, #6493, #753, .T. ) ;
#4406 = CARTESIAN_POINT ( 'NONE',  ( -16.49882833452567965, 99.50000000000000000, 15.05677840364783115 ) ) ;
#4407 = CARTESIAN_POINT ( 'NONE',  ( 9.342627931057743140, 99.50000000000000000, 21.59831790269294771 ) ) ;
#4408 = LINE ( 'NONE', #6808, #7958 ) ;
#4409 = EDGE_CURVE ( 'NONE', #4798, #9216, #3308, .T. ) ;
#4410 = DIRECTION ( 'NONE',  ( 0.000000000000000000, -0.000000000000000000, 1.000000000000000000 ) ) ;
#4411 = CARTESIAN_POINT ( 'NONE',  ( -1.128215178125000273, -1.678124999385482763, -1.954126010382871259 ) ) ;
#4412 = EDGE_LOOP ( 'NONE', ( #6624, #4996, #1550, #5367, #6893 ) ) ;
#4413 = CARTESIAN_POINT ( 'NONE',  ( 4.523042264738025509, 99.50000000000001421, -24.25177047807976294 ) ) ;
#4414 = CARTESIAN_POINT ( 'NONE',  ( 27.43301270000000258, 1.049999998907525267, 0.000000000000000000 ) ) ;
#4415 = CARTESIAN_POINT ( 'NONE',  ( 3.328702480760086235, 99.49999999999997158, -23.35145716610488975 ) ) ;
#4416 = DIRECTION ( 'NONE',  ( -0.000000000000000000, -1.000000000000000000, 0.000000000000000000 ) ) ;
#4417 = VECTOR ( 'NONE', #854, 1000.000000000000114 ) ;
#4418 = EDGE_LOOP ( 'NONE', ( #3945, #6534, #7835, #2416, #7085, #1246, #10336, #3013 ) ) ;
#4419 = EDGE_CURVE ( 'NONE', #5889, #2532, #1634, .T. ) ;
#4420 = CARTESIAN_POINT ( 'NONE',  ( -10.49999999999999822, 104.5000000000000142, 0.000000000000000000 ) ) ;
#4421 = CARTESIAN_POINT ( 'NONE',  ( -16.87593989452418697, 99.99999999999998579, 15.58794934546231126 ) ) ;
#4422 = CARTESIAN_POINT ( 'NONE',  ( -15.15193744131588183, 99.50000000000001421, 16.74589488344418697 ) ) ;
#4423 = EDGE_LOOP ( 'NONE', ( #2758, #6720, #6249, #71 ) ) ;
#4424 = CARTESIAN_POINT ( 'NONE',  ( 4.909381318607588973, 99.50000000000000000, -23.54377677363417121 ) ) ;
#4425 = CARTESIAN_POINT ( 'NONE',  ( -19.39806930854668465, 2.449999998907525622, 19.39806930854667755 ) ) ;
#4426 = CARTESIAN_POINT ( 'NONE',  ( -0.6698729810778043525, -2.286153809338631326, -2.500000000000001332 ) ) ;
#4427 = FACE_OUTER_BOUND ( 'NONE', #4423, .T. ) ;
#4428 = CARTESIAN_POINT ( 'NONE',  ( -21.69499712064247277, 99.99999999999998579, -9.295461156691713356 ) ) ;
#4429 = CARTESIAN_POINT ( 'NONE',  ( 8.961048541867139505, 99.50000000000001421, 19.57961630251783092 ) ) ;
#4430 = CARTESIAN_POINT ( 'NONE',  ( 0.000000000000000000, 100.0000000000000000, 0.000000000000000000 ) ) ;
#4431 = CYLINDRICAL_SURFACE ( 'NONE', #10345, 2.500000000000000000 ) ;
#4432 = CARTESIAN_POINT ( 'NONE',  ( 0.000000000000000000, 0.000000000000000000, 0.000000000000000000 ) ) ;
#4433 = ORIENTED_EDGE ( 'NONE', *, *, #5829, .T. ) ;
#4434 = CARTESIAN_POINT ( 'NONE',  ( -16.49816537377288128, 100.0000000000000000, 16.70951083495554101 ) ) ;
#4435 = CARTESIAN_POINT ( 'NONE',  ( 11.36312591709336139, 2.899999998907526244, -27.43301270000000258 ) ) ;
#4436 = VERTEX_POINT ( 'NONE', #2420 ) ;
#4437 = CARTESIAN_POINT ( 'NONE',  ( 2.500000000000000000, -1.574999999999999734, -3.061616997868383141E-16 ) ) ;
#4438 = EDGE_CURVE ( 'NONE', #4897, #1073, #3668, .T. ) ;
#4439 = CARTESIAN_POINT ( 'NONE',  ( 3.203979444200292015, 99.99999999999997158, -21.29640115293693725 ) ) ;
#4440 = CARTESIAN_POINT ( 'NONE',  ( 2.256430356250000102, -2.278124999385482852, -2.763330213280484622E-16 ) ) ;
#4441 = CARTESIAN_POINT ( 'NONE',  ( 11.36312591709336139, 5.199999998907525622, -27.43301270000000258 ) ) ;
#4442 = CARTESIAN_POINT ( 'NONE',  ( -5.039362679103552881E-15, 0.9499999989075252893, 27.43301270000000258 ) ) ;
#4443 = ORIENTED_EDGE ( 'NONE', *, *, #1477, .T. ) ;
#4444 = UNCERTAINTY_MEASURE_WITH_UNIT (LENGTH_MEASURE( 1.000000000000000082E-05 ), #459, 'distance_accuracy_value', 'NONE');
#4445 = CARTESIAN_POINT ( 'NONE',  ( -15.83671465916681242, 100.0000000000000000, 16.65403364262263608 ) ) ;
#4446 = PLANE ( 'NONE',  #3989 ) ;
#4447 = CARTESIAN_POINT ( 'NONE',  ( -19.09188309203678813, 4.299999997815050712, 19.09188309203678457 ) ) ;
#4448 = CARTESIAN_POINT ( 'NONE',  ( 4.202475441399873723, 100.0000000000000000, -24.35385978717689071 ) ) ;
#4449 = AXIS2_PLACEMENT_3D ( 'NONE', #7992, #8828, #824 ) ;
#4450 = CARTESIAN_POINT ( 'NONE',  ( 1.128215178125001161, -1.790624999385482807, 1.954126010382870815 ) ) ;
#4451 = FACE_OUTER_BOUND ( 'NONE', #8412, .T. ) ;
#4452 = VERTEX_POINT ( 'NONE', #9778 ) ;
#4453 = CARTESIAN_POINT ( 'NONE',  ( 1.128215178124999607, -0.7406249993854828739, -1.954126010382871259 ) ) ;
#4454 = CARTESIAN_POINT ( 'NONE',  ( -5.039362679103552881E-15, 2.449999998907525178, 27.43301270000000258 ) ) ;
#4455 = CARTESIAN_POINT ( 'NONE',  ( -15.17782247516205274, 99.49999999999998579, 15.06300032623928686 ) ) ;
#4456 = EDGE_CURVE ( 'NONE', #9475, #4536, #3434, .T. ) ;
#4457 = CARTESIAN_POINT ( 'NONE',  ( 9.468852706215191262, 99.50000000000000000, 21.22967007823213237 ) ) ;
#4458 = CARTESIAN_POINT ( 'NONE',  ( -17.94007301623892658, 99.50000000000000000, 17.49000340848992607 ) ) ;
#4459 = ORIENTED_EDGE ( 'NONE', *, *, #8874, .T. ) ;
#4460 = ORIENTED_EDGE ( 'NONE', *, *, #8887, .F. ) ;
#4461 = CARTESIAN_POINT ( 'NONE',  ( 9.248677610544923766, 99.50000000000000000, 22.83089001807756446 ) ) ;
#4462 = CARTESIAN_POINT ( 'NONE',  ( 1.128215178124999607, -1.753124999385482718, -1.954126010382871259 ) ) ;
#4463 = ORIENTED_EDGE ( 'NONE', *, *, #3557, .F. ) ;
#4464 = CARTESIAN_POINT ( 'NONE',  ( -22.00707282958688182, 99.99999999999994316, -9.748971510896797810 ) ) ;
#4465 = DIRECTION ( 'NONE',  ( -0.08704561088320925122, 0.9949358851208914833, -0.05025580687519627665 ) ) ;
#4466 = CARTESIAN_POINT ( 'NONE',  ( 0.6698729810778063509, -4.126346188203299903, -2.500000000000000000 ) ) ;
#4467 = CARTESIAN_POINT ( 'NONE',  ( 4.061354557346970040, 99.49999999999997158, -22.84864678426182039 ) ) ;
#4468 = CARTESIAN_POINT ( 'NONE',  ( 9.877377282685029372E-16, -3.037499999999999201, 2.500000000000000000 ) ) ;
#4469 = TOROIDAL_SURFACE ( 'NONE', #9159, 23.82500000000000284, 1.324999999999999956 ) ;
#4470 = CARTESIAN_POINT ( 'NONE',  ( 7.500000000000000000, 104.5000000000000142, -0.9999999999999997780 ) ) ;
#4471 = CARTESIAN_POINT ( 'NONE',  ( -27.00000000000001421, 1.250000000000000222, 11.18376618407356560 ) ) ;
#4472 = CARTESIAN_POINT ( 'NONE',  ( 0.000000000000000000, 97.00000000000000000, -24.00000000000000355 ) ) ;
#4473 = ORIENTED_EDGE ( 'NONE', *, *, #6289, .T. ) ;
#4474 = EDGE_CURVE ( 'NONE', #8554, #6136, #9945, .T. ) ;
#4475 = CARTESIAN_POINT ( 'NONE',  ( 11.18376618407357093, 1.549999997815050490, -27.00000000000000355 ) ) ;
#4476 = CARTESIAN_POINT ( 'NONE',  ( -19.39806930854668465, 4.849999998907525978, 19.39806930854667755 ) ) ;
#4477 = CARTESIAN_POINT ( 'NONE',  ( 2.256430356249999658, -2.578124999385483118, -1.302750673588581432 ) ) ;
#4478 = ADVANCED_FACE ( 'NONE', ( #209 ), #3269, .T. ) ;
#4479 = VECTOR ( 'NONE', #190, 1000.000000000000000 ) ;
#4480 = CARTESIAN_POINT ( 'NONE',  ( -16.63177974700816009, 100.0000000000000000, 16.59747536361813403 ) ) ;
#4481 = ORIENTED_EDGE ( 'NONE', *, *, #5282, .F. ) ;
#4482 = DIRECTION ( 'NONE',  ( 0.000000000000000000, 0.000000000000000000, -1.000000000000000000 ) ) ;
#4483 = CARTESIAN_POINT ( 'NONE',  ( 4.850954546176396320, 99.49999999999998579, -24.43907202982397209 ) ) ;
#4484 = CARTESIAN_POINT ( 'NONE',  ( -0.6698729810778105698, -3.901346188203299814, 2.499999999999997780 ) ) ;
#4485 = CARTESIAN_POINT ( 'NONE',  ( 9.513000527211589841, 99.50000000000000000, 20.35102222961602436 ) ) ;
#4486 = B_SPLINE_CURVE_WITH_KNOTS ( 'NONE', 3,
 ( #6663, #8238, #2552, #9857, #6613, #2694, #7351, #8150, #2643, #1019, #4904, #3332, #4946, #4122, #5834, #285, #8883, #5885, #1845 ),
 .UNSPECIFIED., .F., .F.,
 ( 4, 1, 1, 1, 1, 1, 1, 1, 1, 1, 1, 1, 1, 1, 1, 1, 4 ),
 ( 0.000000000000000000, 0.06282509715607415002, 0.1231380613775250599, 0.1822388757841713336, 0.2396184841454026548, 0.2973605923678978580, 0.3541959668311244203, 0.4122907788200148582, 0.4717534157231769720, 0.5322282553174864095, 0.5926403291039165078, 0.6546871955647078911, 0.7179012776534754448, 0.7839155840457150415, 0.8527518695723632636, 0.9242989153657757972, 1.000000000000000000 ),
 .UNSPECIFIED. ) ;
#4487 = ORIENTED_EDGE ( 'NONE', *, *, #3252, .F. ) ;
#4488 = CARTESIAN_POINT ( 'NONE',  ( -15.37731512048643268, 99.50000000000000000, 15.34394520743122214 ) ) ;
#4489 = DIRECTION ( 'NONE',  ( -0.000000000000000000, 1.000000000000000000, -0.000000000000000000 ) ) ;
#4490 = CARTESIAN_POINT ( 'NONE',  ( 2.500000000000000444, -2.512500000000000178, 1.443375672974063439 ) ) ;
#4491 = APPLICATION_PROTOCOL_DEFINITION ( 'draft international standard', 'automotive_design', 1998, #6203 ) ;
#4492 = CARTESIAN_POINT ( 'NONE',  ( 8.612131858919537919, 99.49999999999998579, 19.96100069886393413 ) ) ;
#4493 = CARTESIAN_POINT ( 'NONE',  ( 3.551917533706515417, 99.50000000000001421, -21.11785906961830150 ) ) ;
#4494 = CARTESIAN_POINT ( 'NONE',  ( -2.256430356250000102, -1.190624999385482941, -1.302750673588580321 ) ) ;
#4495 = CARTESIAN_POINT ( 'NONE',  ( -16.90147242988460263, 99.49999999999998579, 15.68472263728856753 ) ) ;
#4496 = CARTESIAN_POINT ( 'NONE',  ( 27.43301269999999548, 1.099999998907525089, 11.36312591709337738 ) ) ;
#4497 = VERTEX_POINT ( 'NONE', #6684 ) ;
#4498 = CARTESIAN_POINT ( 'NONE',  ( 0.6698729810778087934, -1.932596189432334466, -2.499999999999999112 ) ) ;
#4499 = DIRECTION ( 'NONE',  ( -6.482089281916151093E-13, -1.000000000000000000, -1.430867686834485556E-12 ) ) ;
#4500 = CARTESIAN_POINT ( 'NONE',  ( 3.673732336774000018, 99.50000000000000000, -21.43557726391590279 ) ) ;
#4501 = B_SPLINE_SURFACE_WITH_KNOTS ( 'NONE', 3, 1, ( 
 ( #3657, #7790 ),
 ( #4538, #3868 ),
 ( #4488, #6219 ),
 ( #7735, #6891 ),
 ( #5445, #620 ),
 ( #7054, #2076 ),
 ( #8468, #517 ),
 ( #10088, #10261 ),
 ( #4654, #2924 ),
 ( #10205, #6108 ),
 ( #9299, #8638 ),
 ( #9195, #2015 ),
 ( #8525, #5213 ),
 ( #8413, #4906 ),
 ( #9523, #4704 ),
 ( #8101, #4125 ),
 ( #2505, #7107 ),
 ( #7896, #6428 ),
 ( #5546, #6329 ) ),
 .UNSPECIFIED., .F., .F., .F.,
 ( 4, 1, 1, 1, 1, 1, 1, 1, 1, 1, 1, 1, 1, 1, 1, 1, 4 ),
 ( 2, 2 ),
 ( 0.000000000000000000, 0.06485467887857676583, 0.1277145915909605745, 0.1892127134908106190, 0.2497332716026948729, 0.3109554005383074471, 0.3726238983726959941, 0.4350931267523188151, 0.5000867325104639827, 0.5644742510850394579, 0.6276292343746815439, 0.6888483565510189477, 0.7500704854866314664, 0.8105910435985150819, 0.8724026516570742018, 0.9351453211214243444, 1.000000000000000000 ),
 ( 0.000000000000000000, 1.000000000000000000 ),
 .UNSPECIFIED. ) ;
#4502 = CARTESIAN_POINT ( 'NONE',  ( 3.320270046935387853, 99.99999999999998579, -23.88810568987970484 ) ) ;
#4503 = EDGE_LOOP ( 'NONE', ( #2936, #98 ) ) ;
#4504 = CARTESIAN_POINT ( 'NONE',  ( -2.256430356249998770, -2.353124999385482585, 1.302750673588581876 ) ) ;
#4505 = CARTESIAN_POINT ( 'NONE',  ( 4.820889542125314620, 99.49999999999998579, -21.76289454767624676 ) ) ;
#4506 = EDGE_LOOP ( 'NONE', ( #9987, #1631, #4846, #6958, #5378 ) ) ;
#4507 = CARTESIAN_POINT ( 'NONE',  ( -2.256430356250000102, -0.1781249993854829572, -1.302750673588580321 ) ) ;
#4508 = CARTESIAN_POINT ( 'NONE',  ( 27.43301269999999548, 0.9999999989075252227, 11.36312591709337738 ) ) ;
#4509 = CARTESIAN_POINT ( 'NONE',  ( -15.10737684033046335, 99.50000000000000000, 15.12848924955281049 ) ) ;
#4510 = CARTESIAN_POINT ( 'NONE',  ( -27.00000000000000355, 2.000000000000000000, -3.306546357697854128E-15 ) ) ;
#4511 = DIRECTION ( 'NONE',  ( -0.000000000000000000, -1.000000000000000000, -0.000000000000000000 ) ) ;
#4512 = ORIENTED_EDGE ( 'NONE', *, *, #5762, .T. ) ;
#4513 =( BOUNDED_CURVE ( )  B_SPLINE_CURVE ( 2, ( #8791, #7164, #3927, #6282, #2457 ),
 .UNSPECIFIED., .F., .F. ) 
 B_SPLINE_CURVE_WITH_KNOTS ( ( 3, 2, 3 ),
 ( 0.000000000000000000, 0.01388888888888888812, 0.02083333333333333218 ),
 .UNSPECIFIED. ) 
 CURVE ( )  GEOMETRIC_REPRESENTATION_ITEM ( )  RATIONAL_B_SPLINE_CURVE ( ( 1.000000000000000000, 0.8660254037844387076, 1.000000000000000000, 0.9330127018922194093, 0.9330127018922194093 ) ) 
 REPRESENTATION_ITEM ( '' )  );
#4514 = CARTESIAN_POINT ( 'NONE',  ( 4.852629679480013891, 100.0000000000000142, -23.84752007312514621 ) ) ;
#4515 = CARTESIAN_POINT ( 'NONE',  ( 4.786228327491941173E-16, -2.390624999385482674, 2.605501347177161087 ) ) ;
#4516 = ORIENTED_EDGE ( 'NONE', *, *, #1121, .F. ) ;
#4517 = ADVANCED_FACE ( 'NONE', ( #9937, #9877 ), #412, .F. ) ;
#4518 = CARTESIAN_POINT ( 'NONE',  ( -22.12191435419165941, 99.50000000000001421, -9.834338183724410598 ) ) ;
#4519 = CARTESIAN_POINT ( 'NONE',  ( 2.204364238465235428E-15, 100.0000000000000000, -18.00000000000000000 ) ) ;
#4520 = VECTOR ( 'NONE', #5594, 1000.000000000000114 ) ;
#4521 = CARTESIAN_POINT ( 'NONE',  ( -1.128215178124998497, -0.6281249993854828295, 1.954126010382872147 ) ) ;
#4522 = CARTESIAN_POINT ( 'NONE',  ( 5.226890989224467710, 100.0000000000000284, -23.72545275563321354 ) ) ;
#4523 = DIRECTION ( 'NONE',  ( -0.000000000000000000, -1.000000000000000000, -0.000000000000000000 ) ) ;
#4524 = FACE_OUTER_BOUND ( 'NONE', #4412, .T. ) ;
#4525 = CARTESIAN_POINT ( 'NONE',  ( 2.500000000000000444, -2.962499999999999911, 1.443375672974063439 ) ) ;
#4526 = EDGE_LOOP ( 'NONE', ( #5095, #6153, #3790, #619 ) ) ;
#4527 = DIRECTION ( 'NONE',  ( 0.000000000000000000, -1.000000000000000000, 0.000000000000000000 ) ) ;
#4528 = CARTESIAN_POINT ( 'NONE',  ( -0.6698729810778020211, -4.536153809338631326, -2.500000000000002665 ) ) ;
#4529 = CARTESIAN_POINT ( 'NONE',  ( 1.128215178124999607, -2.090624999385482852, -1.954126010382871259 ) ) ;
#4530 = CARTESIAN_POINT ( 'NONE',  ( 9.861577898019769250, 99.99999999999994316, 21.03794551367759169 ) ) ;
#4531 = ORIENTED_EDGE ( 'NONE', *, *, #6072, .F. ) ;
#4532 = CARTESIAN_POINT ( 'NONE',  ( 8.685676809262872666, 99.50000000000000000, 23.43455588346217766 ) ) ;
#4533 = DIRECTION ( 'NONE',  ( 0.000000000000000000, -0.000000000000000000, -1.000000000000000000 ) ) ;
#4534 = ADVANCED_FACE ( 'NONE', ( #5962 ), #1769, .T. ) ;
#4535 = DIRECTION ( 'NONE',  ( 0.000000000000000000, -0.000000000000000000, 1.000000000000000000 ) ) ;
#4536 = VERTEX_POINT ( 'NONE', #993 ) ;
#4537 = EDGE_CURVE ( 'NONE', #1184, #341, #10157, .T. ) ;
#4538 = CARTESIAN_POINT ( 'NONE',  ( -15.34161522349497808, 99.49999999999998579, 15.37783959465231121 ) ) ;
#4539 = VECTOR ( 'NONE', #4698, 1000.000000000000227 ) ;
#4540 = FACE_OUTER_BOUND ( 'NONE', #10031, .T. ) ;
#4541 = VECTOR ( 'NONE', #1822, 1000.000000000000000 ) ;
#4542 = VERTEX_POINT ( 'NONE', #1466 ) ;
#4543 = CARTESIAN_POINT ( 'NONE',  ( 2.500000000000000000, -2.437500000000000000, -1.443375672974064994 ) ) ;
#4544 = ADVANCED_FACE ( 'NONE', ( #1355 ), #8530, .T. ) ;
#4545 = CARTESIAN_POINT ( 'NONE',  ( 0.000000000000000000, 0.000000000000000000, 0.000000000000000000 ) ) ;
#4546 = DIRECTION ( 'NONE',  ( -0.8660254037844393737, 0.4999999999999986677, 0.000000000000000000 ) ) ;
#4547 = CARTESIAN_POINT ( 'NONE',  ( 0.6698729810778063509, -3.732596189432333844, -2.500000000000000000 ) ) ;
#4548 = CARTESIAN_POINT ( 'NONE',  ( 4.786228327491941173E-16, -2.390624999385482674, 2.605501347177161087 ) ) ;
#4549 = CARTESIAN_POINT ( 'NONE',  ( -16.70213339477928471, 99.49999999999998579, 16.52464093453885852 ) ) ;
#4550 = CARTESIAN_POINT ( 'NONE',  ( -19.39806930854668465, 3.249999998907525001, 19.39806930854667755 ) ) ;
#4551 = ORIENTED_EDGE ( 'NONE', *, *, #9899, .T. ) ;
#4552 = AXIS2_PLACEMENT_3D ( 'NONE', #6619, #3591, #344 ) ;
#4553 = CARTESIAN_POINT ( 'NONE',  ( 9.357053078540884528, 100.0000000000000142, 19.70216357796830664 ) ) ;
#4554 = CARTESIAN_POINT ( 'NONE',  ( -19.46743691185369585, 100.0000000000000000, -8.912588186774021537 ) ) ;
#4555 = CARTESIAN_POINT ( 'NONE',  ( -3.000000000000000888, -15.00000000000000000, -1.732050807568877415 ) ) ;
#4556 = EDGE_CURVE ( 'NONE', #1808, #2926, #2837, .T. ) ;
#4557 = CYLINDRICAL_SURFACE ( 'NONE', #6618, 2.500000000000000000 ) ;
#4558 = CARTESIAN_POINT ( 'NONE',  ( -2.256430356250000102, -1.040624999385483029, 0.000000000000000000 ) ) ;
#4559 = DIRECTION ( 'NONE',  ( -0.000000000000000000, -1.000000000000000000, -0.000000000000000000 ) ) ;
#4560 = ORIENTED_EDGE ( 'NONE', *, *, #5048, .T. ) ;
#4561 = DIRECTION ( 'NONE',  ( 0.000000000000000000, -0.000000000000000000, 1.000000000000000000 ) ) ;
#4562 = CARTESIAN_POINT ( 'NONE',  ( -27.43301270000000258, 2.249999998907525001, -3.359575119402369376E-15 ) ) ;
#4563 =( NAMED_UNIT ( * ) PLANE_ANGLE_UNIT ( ) SI_UNIT ( $, .RADIAN. ) );
#4564 = EDGE_LOOP ( 'NONE', ( #4354, #4385, #10015, #612 ) ) ;
#4565 = B_SPLINE_CURVE_WITH_KNOTS ( 'NONE', 3,
 ( #4396, #6067, #9258, #9998, #2089, #3560, #7635, #9106, #8482, #4243, #1927, #1152, #5124, #6015, #7424, #1876, #266, #5227, #3455 ),
 .UNSPECIFIED., .F., .F.,
 ( 4, 1, 1, 1, 1, 1, 1, 1, 1, 1, 1, 1, 1, 1, 1, 1, 4 ),
 ( 0.000000000000000000, 0.06839333837245492598, 0.1346519561570838353, 0.1985335841112251809, 0.2613354512981445610, 0.3228799447584090876, 0.3842093944964607433, 0.4462111754260434937, 0.5089246482083435996, 0.5715029624870164859, 0.6324491702983550123, 0.6923675070709934820, 0.7521785462597534444, 0.8119602890481165680, 0.8728645645504365946, 0.9355733815441056311, 1.000000000000000000 ),
 .UNSPECIFIED. ) ;
#4566 = CARTESIAN_POINT ( 'NONE',  ( -20.96643530928959365, 99.50000000000000000, -10.05541671241504886 ) ) ;
#4567 = CARTESIAN_POINT ( 'NONE',  ( -27.00000000000000355, 1.150000000000000133, -11.18376618407357093 ) ) ;
#4568 = DIRECTION ( 'NONE',  ( 0.000000000000000000, -1.000000000000000000, 0.000000000000000000 ) ) ;
#4569 = VERTEX_POINT ( 'NONE', #8589 ) ;
#4570 = CARTESIAN_POINT ( 'NONE',  ( -19.09188309203678457, 2.700000000000000178, -19.09188309203678813 ) ) ;
#4571 = CARTESIAN_POINT ( 'NONE',  ( 8.074269155311188939, 100.0000000000000142, 20.56111086218762551 ) ) ;
#4572 = VECTOR ( 'NONE', #291, 1000.000000000000000 ) ;
#4573 = CARTESIAN_POINT ( 'NONE',  ( 2.256430356249999658, -3.590624999385481964, -1.302750673588581432 ) ) ;
#4574 = ORIENTED_EDGE ( 'NONE', *, *, #7111, .T. ) ;
#4575 = ORIENTED_EDGE ( 'NONE', *, *, #7297, .T. ) ;
#4576 = LINE ( 'NONE', #9960, #8809 ) ;
#4577 = CARTESIAN_POINT ( 'NONE',  ( 0.000000000000000000, -5.000000000000000000, -2.499999999999999556 ) ) ;
#4578 = CARTESIAN_POINT ( 'NONE',  ( 1.128215178124999607, -0.4031249993854829627, -1.954126010382871259 ) ) ;
#4579 = CARTESIAN_POINT ( 'NONE',  ( 3.080354370726382296, 100.0000000000000426, -23.09295995363041598 ) ) ;
#4580 = ADVANCED_FACE ( 'NONE', ( #5276 ), #7006, .T. ) ;
#4581 = CARTESIAN_POINT ( 'NONE',  ( 4.486604876299897349, 99.50000000000000000, -21.85617661337775885 ) ) ;
#4582 = CARTESIAN_POINT ( 'NONE',  ( -17.94007301623892658, 100.0000000000000000, 17.49000340848992607 ) ) ;
#4583 = DIRECTION ( 'NONE',  ( 0.000000000000000000, 0.000000000000000000, 1.000000000000000000 ) ) ;
#4584 = FACE_OUTER_BOUND ( 'NONE', #3410, .T. ) ;
#4585 = ORIENTED_EDGE ( 'NONE', *, *, #3307, .F. ) ;
#4586 = LINE ( 'NONE', #5489, #1556 ) ;
#4587 = CARTESIAN_POINT ( 'NONE',  ( 2.256430356249999658, -2.128124999385482941, -1.302750673588581432 ) ) ;
#4588 = AXIS2_PLACEMENT_3D ( 'NONE', #10332, #4878, #4044 ) ;
#4589 = EDGE_CURVE ( 'NONE', #9350, #4614, #8783, .T. ) ;
#4590 = B_SPLINE_SURFACE_WITH_KNOTS ( 'NONE', 3, 1, ( 
 ( #4816, #7959 ),
 ( #792, #3983 ),
 ( #8796, #1621 ),
 ( #8012, #8848 ),
 ( #8255, #1084 ),
 ( #3435, #201 ),
 ( #1760, #1811 ) ),
 .UNSPECIFIED., .F., .F., .F.,
 ( 4, 1, 1, 1, 4 ),
 ( 2, 2 ),
 ( 0.000000000000000000, 0.2676680225848128147, 0.5230972062070123885, 0.7658030722156558001, 1.000000000000000000 ),
 ( 0.000000000000000000, 1.000000000000000000 ),
 .UNSPECIFIED. ) ;
#4591 = ORIENTED_EDGE ( 'NONE', *, *, #5314, .T. ) ;
#4592 = CARTESIAN_POINT ( 'NONE',  ( -20.95972469638759250, 100.0000000000000000, -9.536167108072199028 ) ) ;
#4593 = CARTESIAN_POINT ( 'NONE',  ( 9.063633472794011325, 99.99999999999998579, 19.59517414759687526 ) ) ;
#4594 = DIRECTION ( 'NONE',  ( 1.000000000000000000, 0.000000000000000000, 0.000000000000000000 ) ) ;
#4595 = CARTESIAN_POINT ( 'NONE',  ( -16.57337958714257908, 99.49999999999998579, 15.99273699073067867 ) ) ;
#4596 = VERTEX_POINT ( 'NONE', #5451 ) ;
#4597 = CARTESIAN_POINT ( 'NONE',  ( -16.49816537377288128, 99.50000000000000000, 16.70951083495554101 ) ) ;
#4598 = CARTESIAN_POINT ( 'NONE',  ( 11.36312591709336850, 0.9999999989075253337, 27.43301269999999903 ) ) ;
#4599 = ORIENTED_EDGE ( 'NONE', *, *, #10245, .T. ) ;
#4600 = APPLICATION_CONTEXT ( 'automotive_design' ) ;
#4601 = CARTESIAN_POINT ( 'NONE',  ( -1.250000000000000222, -4.124999999999999112, -2.165063509461096825 ) ) ;
#4602 = VECTOR ( 'NONE', #5895, 1000.000000000000000 ) ;
#4603 = CARTESIAN_POINT ( 'NONE',  ( 3.681717055787076642, 99.50000000000000000, -21.09125273517263111 ) ) ;
#4604 = CARTESIAN_POINT ( 'NONE',  ( -1.595409442497313560E-16, -3.065624999385482496, -2.605501347177161087 ) ) ;
#4605 = CARTESIAN_POINT ( 'NONE',  ( 27.00000000000000355, 0.6499999978150503566, -11.18376618407356915 ) ) ;
#4606 = CARTESIAN_POINT ( 'NONE',  ( 27.43301270000000258, 3.599999998907525534, -11.36312591709336139 ) ) ;
#4607 = CARTESIAN_POINT ( 'NONE',  ( -15.42740294075255925, 100.0000000000000000, 14.91894146668702348 ) ) ;
#4608 = CARTESIAN_POINT ( 'NONE',  ( 0.000000000000000000, 0.000000000000000000, 0.000000000000000000 ) ) ;
#4609 = CARTESIAN_POINT ( 'NONE',  ( 3.202955020264580899, 99.50000000000000000, -21.91595956354277064 ) ) ;
#4610 = AXIS2_PLACEMENT_3D ( 'NONE', #4291, #4191, #7422 ) ;
#4611 = CARTESIAN_POINT ( 'NONE',  ( -15.98972951825121669, 99.99999999999997158, 15.19400804711857411 ) ) ;
#4612 = CARTESIAN_POINT ( 'NONE',  ( -2.256430356250000102, -1.490624999385482763, 0.000000000000000000 ) ) ;
#4613 = CARTESIAN_POINT ( 'NONE',  ( 4.034460619503033030, 99.49999999999995737, -21.08676866017170681 ) ) ;
#4614 = VERTEX_POINT ( 'NONE', #6843 ) ;
#4615 = ORIENTED_EDGE ( 'NONE', *, *, #3557, .T. ) ;
#4616 = CARTESIAN_POINT ( 'NONE',  ( -2.256430356250000102, -2.878124999385482941, -1.302750673588580321 ) ) ;
#4617 = CIRCLE ( 'NONE', #5623, 18.00000000000000000 ) ;
#4618 = CARTESIAN_POINT ( 'NONE',  ( -19.39806930854667755, 2.949999998907525178, -19.39806930854668110 ) ) ;
#4619 = ADVANCED_FACE ( 'NONE', ( #8418 ), #2082, .T. ) ;
#4620 =( NAMED_UNIT ( * ) SI_UNIT ( $, .STERADIAN. ) SOLID_ANGLE_UNIT ( ) );
#4621 = ORIENTED_EDGE ( 'NONE', *, *, #2294, .F. ) ;
#4622 = CARTESIAN_POINT ( 'NONE',  ( 0.000000000000000000, 71.18660744634364335, 0.000000000000000000 ) ) ;
#4623 = EDGE_CURVE ( 'NONE', #1444, #3142, #2023, .T. ) ;
#4624 = CARTESIAN_POINT ( 'NONE',  ( 26.99999999999999645, 2.350000000000000533, 11.18376618407358691 ) ) ;
#4625 = CARTESIAN_POINT ( 'NONE',  ( 9.114876806416853938, 99.49999999999998579, 19.97295714941878231 ) ) ;
#4626 = ORIENTED_EDGE ( 'NONE', *, *, #624, .F. ) ;
#4627 = CARTESIAN_POINT ( 'NONE',  ( -16.57687742313193269, 99.50000000000002842, 15.91855687263828756 ) ) ;
#4628 = DIRECTION ( 'NONE',  ( 0.000000000000000000, -1.000000000000000000, 0.000000000000000000 ) ) ;
#4629 = ORIENTED_EDGE ( 'NONE', *, *, #8891, .F. ) ;
#4630 = CARTESIAN_POINT ( 'NONE',  ( -1.595409442497313560E-16, -4.415624999385482141, -2.605501347177161087 ) ) ;
#4631 = VERTEX_POINT ( 'NONE', #1410 ) ;
#4632 = DIRECTION ( 'NONE',  ( 0.000000000000000000, -1.000000000000000000, 0.000000000000000000 ) ) ;
#4633 = CARTESIAN_POINT ( 'NONE',  ( 0.6698729810778065730, -0.1325961894323341994, -2.499999999999999556 ) ) ;
#4634 = AXIS2_PLACEMENT_3D ( 'NONE', #5085, #8976, #4989 ) ;
#4635 = CARTESIAN_POINT ( 'NONE',  ( -2.256430356250000102, -1.190624999385482941, -1.302750673588580321 ) ) ;
#4636 = CARTESIAN_POINT ( 'NONE',  ( 3.058419780146050648, 100.0000000000000000, -23.12871267107006545 ) ) ;
#4637 = CARTESIAN_POINT ( 'NONE',  ( -2.499999999999999112, -1.762499999999999734, 1.443375672974065882 ) ) ;
#4638 = AXIS2_PLACEMENT_3D ( 'NONE', #6907, #3051, #10105 ) ;
#4639 = CARTESIAN_POINT ( 'NONE',  ( -2.500000000000000000, -1.781249998770965570, -1.443375672974064106 ) ) ;
#4640 = CARTESIAN_POINT ( 'NONE',  ( 4.640952353770416927, 100.0000000000000142, -24.17064508475253604 ) ) ;
#4641 = CARTESIAN_POINT ( 'NONE',  ( 0.000000000000000000, 5.000000000000000000, 0.000000000000000000 ) ) ;
#4642 = ORIENTED_EDGE ( 'NONE', *, *, #5762, .F. ) ;
#4643 = LINE ( 'NONE', #7836, #7534 ) ;
#4644 =( BOUNDED_CURVE ( )  B_SPLINE_CURVE ( 2, ( #7384, #1785, #3713, #6896, #7338, #222, #1882, #5027, #9065 ),
 .UNSPECIFIED., .F., .T. ) 
 B_SPLINE_CURVE_WITH_KNOTS ( ( 3, 2, 2, 2, 3 ),
 ( 0.3541666666666666852, 0.3611111111111111049, 0.3750000000000000000, 0.3888888888888888951, 0.3958333333333333703 ),
 .UNSPECIFIED. ) 
 CURVE ( )  GEOMETRIC_REPRESENTATION_ITEM ( )  RATIONAL_B_SPLINE_CURVE ( ( 0.9330127018922194093, 0.9330127018922196314, 1.000000000000000000, 0.8660254037844387076, 1.000000000000000000, 0.8660254037844387076, 1.000000000000000000, 0.9330127018922190762, 0.9330127018922194093 ) ) 
 REPRESENTATION_ITEM ( '' )  );
#4645 = CARTESIAN_POINT ( 'NONE',  ( -2.256430356250000102, -1.528124999385482630, -1.302750673588580321 ) ) ;
#4646 = CARTESIAN_POINT ( 'NONE',  ( -21.13504512532655610, 100.0000000000000000, -11.31853095674525100 ) ) ;
#4647 = VERTEX_POINT ( 'NONE', #2932 ) ;
#4648 = FACE_OUTER_BOUND ( 'NONE', #3796, .T. ) ;
#4649 = CARTESIAN_POINT ( 'NONE',  ( 8.536201443755420115, 100.0000000000000284, 19.63502355897212581 ) ) ;
#4650 = CYLINDRICAL_SURFACE ( 'NONE', #9705, 23.99999999999999645 ) ;
#4651 = LINE ( 'NONE', #8686, #6651 ) ;
#4652 = EDGE_LOOP ( 'NONE', ( #4516, #2587, #5419, #6353 ) ) ;
#4653 = B_SPLINE_CURVE_WITH_KNOTS ( 'NONE', 3,
 ( #849, #8293, #4087, #9634, #6771, #56, #3530, #2469, #1953, #5941, #8853, #6666, #4039, #1124, #7272 ),
 .UNSPECIFIED., .F., .F.,
 ( 4, 1, 1, 1, 1, 1, 1, 1, 1, 1, 1, 1, 4 ),
 ( 0.000000000000000000, 0.09895296010982183865, 0.1966578232739713550, 0.2939931048315790330, 0.3929322324600736938, 0.4463669803336778319, 0.5055752425223922764, 0.5715235163887821823, 0.6440401046887170855, 0.7229629404452876384, 0.8087840669208056221, 0.9009145765370688563, 1.000000000000000000 ),
 .UNSPECIFIED. ) ;
#4654 = CARTESIAN_POINT ( 'NONE',  ( -15.76955986605724647, 99.49999999999998579, 15.18352214517458698 ) ) ;
#4655 = CARTESIAN_POINT ( 'NONE',  ( 11.36312591709336850, 3.399999998907525356, 27.43301269999999903 ) ) ;
#4656 = ORIENTED_EDGE ( 'NONE', *, *, #3264, .F. ) ;
#4657 = ADVANCED_FACE ( 'NONE', ( #6224 ), #6270, .T. ) ;
#4658 = FILL_AREA_STYLE_COLOUR ( '', #4393 ) ;
#4659 = CARTESIAN_POINT ( 'NONE',  ( 0.6698729810778025762, -3.917403810567665623, 2.500000000000002665 ) ) ;
#4660 = CARTESIAN_POINT ( 'NONE',  ( 2.256430356250000102, -1.828124999385482674, -2.763330213280484622E-16 ) ) ;
#4661 = CARTESIAN_POINT ( 'NONE',  ( -16.65546786808457469, 99.49999999999998579, 16.57295196178722918 ) ) ;
#4662 = CARTESIAN_POINT ( 'NONE',  ( 27.43301270000000258, 1.199999998907525178, -11.36312591709336139 ) ) ;
#4663 = ORIENTED_EDGE ( 'NONE', *, *, #8315, .T. ) ;
#4664 = PRODUCT_DEFINITION_CONTEXT ( 'detailed design', #2467, 'design' ) ;
#4665 = CARTESIAN_POINT ( 'NONE',  ( -15.22320097062094568, 99.50000000000001421, 16.32303119091969634 ) ) ;
#4666 = CARTESIAN_POINT ( 'NONE',  ( 3.970307086022987431, 99.50000000000001421, -24.36314111580913178 ) ) ;
#4667 = DIRECTION ( 'NONE',  ( 0.8660254037844385966, 0.000000000000000000, -0.5000000000000000000 ) ) ;
#4668 = DIRECTION ( 'NONE',  ( 0.000000000000000000, 0.000000000000000000, -1.000000000000000000 ) ) ;
#4669 = CARTESIAN_POINT ( 'NONE',  ( 1.128215178124999607, -2.090624999385482852, -1.954126010382871259 ) ) ;
#4670 = CARTESIAN_POINT ( 'NONE',  ( 3.771794781161601939, 99.99999999999998579, -21.07813736596861176 ) ) ;
#4671 = ORIENTED_EDGE ( 'NONE', *, *, #237, .F. ) ;
#4672 = EDGE_CURVE ( 'NONE', #405, #7350, #6311, .T. ) ;
#4673 = CARTESIAN_POINT ( 'NONE',  ( -1.128215178125000273, -1.565624999385482941, -1.954126010382871259 ) ) ;
#4674 = CARTESIAN_POINT ( 'NONE',  ( -27.43301270000000258, 2.199999998907525622, -11.36312591709336317 ) ) ;
#4675 = DIRECTION ( 'NONE',  ( -0.000000000000000000, -1.000000000000000000, -0.000000000000000000 ) ) ;
#4676 = EDGE_LOOP ( 'NONE', ( #1284, #9665 ) ) ;
#4677 = CARTESIAN_POINT ( 'NONE',  ( 7.826802610544922878, 100.0000000000000000, 21.21129867192371421 ) ) ;
#4678 = CARTESIAN_POINT ( 'NONE',  ( 8.564701892180647036, 99.50000000000000000, 19.97971282122689018 ) ) ;
#4679 = VERTEX_POINT ( 'NONE', #3292 ) ;
#4680 = CARTESIAN_POINT ( 'NONE',  ( -15.11748654497029953, 99.49999999999998579, 15.76872032455190897 ) ) ;
#4681 = CARTESIAN_POINT ( 'NONE',  ( 8.063732359723156051, 99.50000000000001421, 20.72384750152746236 ) ) ;
#4682 = EDGE_CURVE ( 'NONE', #3916, #8960, #9035, .T. ) ;
#4683 = EDGE_LOOP ( 'NONE', ( #2788, #4919, #4365, #6190 ) ) ;
#4684 = CARTESIAN_POINT ( 'NONE',  ( 4.786228327491941173E-16, -4.190624999385482496, 2.605501347177161087 ) ) ;
#4685 = ORIENTED_EDGE ( 'NONE', *, *, #651, .F. ) ;
#4686 = EDGE_CURVE ( 'NONE', #1838, #7872, #4513, .T. ) ;
#4687 = CARTESIAN_POINT ( 'NONE',  ( 19.39806930854668110, 1.949999998907525178, -19.39806930854668110 ) ) ;
#4688 = CARTESIAN_POINT ( 'NONE',  ( -21.45221949983897858, 99.50000000000000000, -9.661157428473494235 ) ) ;
#4689 = B_SPLINE_SURFACE_WITH_KNOTS ( 'NONE', 3, 1, ( 
 ( #7933, #4480 ),
 ( #767, #5204 ),
 ( #10348, #2006 ),
 ( #3958, #6364 ),
 ( #9558, #2387 ),
 ( #5582, #3592 ),
 ( #1234, #4982 ),
 ( #964, #5631 ),
 ( #8821, #1696 ),
 ( #1597, #8919 ),
 ( #8036, #1010 ),
 ( #9653, #1650 ),
 ( #175, #4788 ),
 ( #2490, #869 ),
 ( #8969, #8180 ),
 ( #8088, #5683 ),
 ( #4893, #4201 ),
 ( #4010, #4158 ),
 ( #9700, #7385 ) ),
 .UNSPECIFIED., .F., .F., .F.,
 ( 4, 1, 1, 1, 1, 1, 1, 1, 1, 1, 1, 1, 1, 1, 1, 1, 4 ),
 ( 2, 2 ),
 ( 0.000000000000000000, 0.06363772181477481138, 0.1253661190162797812, 0.1854850957718461035, 0.2454326483351531030, 0.3054881917026986415, 0.3659564384638642753, 0.4275766838088623234, 0.4913505196498278993, 0.5556437034595619329, 0.6183735394983103095, 0.6802114403575724166, 0.7422401234104337719, 0.8041288543812358247, 0.8678488776753463529, 0.9326351893241184854, 1.000000000000000000 ),
 ( 0.000000000000000000, 1.000000000000000000 ),
 .UNSPECIFIED. ) ;
#4690 = CARTESIAN_POINT ( 'NONE',  ( -1.128215178124998497, -2.428124999385482763, 1.954126010382872147 ) ) ;
#4691 = CARTESIAN_POINT ( 'NONE',  ( 4.922541232168287983, 99.50000000000002842, -24.37252920941159928 ) ) ;
#4692 = CARTESIAN_POINT ( 'NONE',  ( 1.653273178848927064E-15, 4.799999997815051600, -27.00000000000000355 ) ) ;
#4693 = CARTESIAN_POINT ( 'NONE',  ( 1.250000000000001110, -2.493749998770965703, 2.165063509461096380 ) ) ;
#4694 = VERTEX_POINT ( 'NONE', #8843 ) ;
#4695 = CARTESIAN_POINT ( 'NONE',  ( 4.739008722453743161, 99.50000000000000000, -24.06821587619827341 ) ) ;
#4696 = CARTESIAN_POINT ( 'NONE',  ( -20.66709314808276332, 99.50000000000002842, -10.01107456535036455 ) ) ;
#4697 = ORIENTED_EDGE ( 'NONE', *, *, #2750, .T. ) ;
#4698 = DIRECTION ( 'NONE',  ( -0.3368610894541371747, 0.000000000000000000, 0.9415543565890243105 ) ) ;
#4699 = CARTESIAN_POINT ( 'NONE',  ( 2.256430356250000102, -2.165624999385483029, -2.763330213280484622E-16 ) ) ;
#4700 = CARTESIAN_POINT ( 'NONE',  ( -22.33529725360453000, 99.99999999999997158, -10.20112572733487255 ) ) ;
#4701 = CARTESIAN_POINT ( 'NONE',  ( 9.600410285814406919, 99.99999999999998579, 19.87914582625927196 ) ) ;
#4702 = DIRECTION ( 'NONE',  ( -0.000000000000000000, 1.000000000000000000, -0.000000000000000000 ) ) ;
#4703 = VERTEX_POINT ( 'NONE', #9976 ) ;
#4704 = CARTESIAN_POINT ( 'NONE',  ( -16.18965924272485779, 99.99999999999998579, 15.26525457555968224 ) ) ;
#4705 = CARTESIAN_POINT ( 'NONE',  ( 27.43301270000000258, 3.549999998907525267, 0.000000000000000000 ) ) ;
#4706 = ORIENTED_EDGE ( 'NONE', *, *, #5641, .T. ) ;
#4707 = CARTESIAN_POINT ( 'NONE',  ( 2.500000000000000444, -3.862499999999999822, 1.443375672974063439 ) ) ;
#4708 = CARTESIAN_POINT ( 'NONE',  ( 3.293841816516395848, 99.49999999999998579, -23.44781013845121009 ) ) ;
#4709 = CARTESIAN_POINT ( 'NONE',  ( -1.128215178125000273, -4.828124999385481786, -1.954126010382871259 ) ) ;
#4710 = CARTESIAN_POINT ( 'NONE',  ( 3.764204346677844093, 100.0000000000000426, -22.52576385118515745 ) ) ;
#4711 = CARTESIAN_POINT ( 'NONE',  ( -27.00000000000000355, 1.749999997815050667, -11.18376618407357093 ) ) ;
#4712 = ADVANCED_FACE ( 'NONE', ( #1669 ), #9455, .T. ) ;
#4713 = CARTESIAN_POINT ( 'NONE',  ( -15.13520964245927836, 99.99999999999995737, 15.69931698147095034 ) ) ;
#4714 = CARTESIAN_POINT ( 'NONE',  ( 3.286905236079108672, 100.0000000000000426, -23.77014634954566574 ) ) ;
#4715 = CARTESIAN_POINT ( 'NONE',  ( 3.446946945638383664, 99.49999999999997158, -21.53774374131874580 ) ) ;
#4716 = CARTESIAN_POINT ( 'NONE',  ( -22.59920249870969045, 99.99999999999998579, -10.80326527670058567 ) ) ;
#4717 = CARTESIAN_POINT ( 'NONE',  ( -2.256430356250000102, -3.740624999385482763, 0.000000000000000000 ) ) ;
#4718 = CARTESIAN_POINT ( 'NONE',  ( -21.11719860449141351, 99.50000000000002842, -9.425423427278841970 ) ) ;
#4719 = ORIENTED_EDGE ( 'NONE', *, *, #319, .F. ) ;
#4720 = VERTEX_POINT ( 'NONE', #9088 ) ;
#4721 = CARTESIAN_POINT ( 'NONE',  ( 2.256430356250000102, -3.065624999385482496, -2.763330213280484622E-16 ) ) ;
#4722 = CARTESIAN_POINT ( 'NONE',  ( -19.39806930854667755, 4.549999998907525267, -19.39806930854668110 ) ) ;
#4723 = CARTESIAN_POINT ( 'NONE',  ( -16.38049141020750099, 99.50000000000004263, 14.97568473612765416 ) ) ;
#4724 = CARTESIAN_POINT ( 'NONE',  ( 11.18376618407356915, 0.1499999999999999944, -27.00000000000000355 ) ) ;
#4725 = CYLINDRICAL_SURFACE ( 'NONE', #2029, 27.00000000000000355 ) ;
#4726 = EDGE_CURVE ( 'NONE', #2231, #957, #350, .T. ) ;
#4727 = EDGE_CURVE ( 'NONE', #533, #5515, #8168, .T. ) ;
#4728 = CARTESIAN_POINT ( 'NONE',  ( 1.249999999999999334, -3.299999999999999378, -2.165063509461096825 ) ) ;
#4729 = CARTESIAN_POINT ( 'NONE',  ( 8.149445629999579666, 99.50000000000002842, 20.33980848884064230 ) ) ;
#4730 = VERTEX_POINT ( 'NONE', #9816 ) ;
#4731 = CARTESIAN_POINT ( 'NONE',  ( 1.128215178125001161, -3.703124999385482230, 1.954126010382870815 ) ) ;
#4732 = VERTEX_POINT ( 'NONE', #2651 ) ;
#4733 = CARTESIAN_POINT ( 'NONE',  ( -19.39806930854668465, 2.349999998907525534, 19.39806930854667755 ) ) ;
#4734 = CARTESIAN_POINT ( 'NONE',  ( 4.135809822336132591, 99.49999999999998579, -24.70305975188825443 ) ) ;
#4735 = CARTESIAN_POINT ( 'NONE',  ( 0.000000000000000000, 100.0000000000000000, 0.000000000000000000 ) ) ;
#4736 = CARTESIAN_POINT ( 'NONE',  ( -1.128215178125000273, -1.678124999385482763, -1.954126010382871259 ) ) ;
#4737 = CARTESIAN_POINT ( 'NONE',  ( 5.825495487346713297, 99.50000000000000000, 20.69456627699299744 ) ) ;
#4738 = FACE_OUTER_BOUND ( 'NONE', #9365, .T. ) ;
#4739 = CARTESIAN_POINT ( 'NONE',  ( 4.472992770554171216, 99.49999999999998579, -21.83386288566719458 ) ) ;
#4740 =( GEOMETRIC_REPRESENTATION_CONTEXT ( 3 ) GLOBAL_UNCERTAINTY_ASSIGNED_CONTEXT ( ( #5402 ) ) GLOBAL_UNIT_ASSIGNED_CONTEXT ( ( #9623, #4862, #3291 ) ) REPRESENTATION_CONTEXT ( 'NONE', 'WORKASPACE' ) );
#4741 = CARTESIAN_POINT ( 'NONE',  ( -1.249999999999998224, -2.118749998770965703, 2.165063509461097713 ) ) ;
#4742 = ORIENTED_EDGE ( 'NONE', *, *, #3277, .T. ) ;
#4743 = CARTESIAN_POINT ( 'NONE',  ( 4.640952353770416927, 99.50000000000000000, -24.17064508475253604 ) ) ;
#4744 = CARTESIAN_POINT ( 'NONE',  ( -9.703070624755296135E-15, -4.331249998770966059, 2.500000000000000444 ) ) ;
#4745 = CARTESIAN_POINT ( 'NONE',  ( 2.256430356249999658, -3.478124999385482585, -1.302750673588581432 ) ) ;
#4746 = VERTEX_POINT ( 'NONE', #9036 ) ;
#4747 = ORIENTED_EDGE ( 'NONE', *, *, #2997, .F. ) ;
#4748 = EDGE_CURVE ( 'NONE', #4798, #3656, #7776, .T. ) ;
#4749 = DIRECTION ( 'NONE',  ( -1.224646799147353207E-16, 0.000000000000000000, -1.000000000000000000 ) ) ;
#4750 = SURFACE_STYLE_FILL_AREA ( #3919 ) ;
#4751 = CARTESIAN_POINT ( 'NONE',  ( -22.33529725360453000, 99.49999999999997158, -10.20112572733487255 ) ) ;
#4752 = CARTESIAN_POINT ( 'NONE',  ( -15.07178375341841381, 99.50000000000000000, 16.66969090848992607 ) ) ;
#4753 = CARTESIAN_POINT ( 'NONE',  ( 27.43301270000000258, 5.149999998907525800, 0.000000000000000000 ) ) ;
#4754 = ORIENTED_EDGE ( 'NONE', *, *, #7781, .F. ) ;
#4755 = CARTESIAN_POINT ( 'NONE',  ( 2.500000000000000000, -3.337499999999999467, -1.443375672974064994 ) ) ;
#4756 = CARTESIAN_POINT ( 'NONE',  ( 3.222930479149370253, 99.99999999999995737, -22.15251218086615381 ) ) ;
#4757 = CARTESIAN_POINT ( 'NONE',  ( 2.256430356249999658, -4.040624999385483029, -1.302750673588581432 ) ) ;
#4758 = CARTESIAN_POINT ( 'NONE',  ( -20.89948324804827706, 99.50000000000001421, -10.26098411820691858 ) ) ;
#4759 = CARTESIAN_POINT ( 'NONE',  ( -11.18376618407358336, 1.149999997815050357, 26.99999999999999645 ) ) ;
#4760 = UNCERTAINTY_MEASURE_WITH_UNIT (LENGTH_MEASURE( 1.000000000000000082E-05 ), #6296, 'distance_accuracy_value', 'NONE');
#4761 = CARTESIAN_POINT ( 'NONE',  ( -15.11748654497029953, 99.49999999999998579, 15.76872032455190897 ) ) ;
#4762 = CARTESIAN_POINT ( 'NONE',  ( 21.82251602564102910, 99.50000000000000000, -0.5181290064102563875 ) ) ;
#4763 = CARTESIAN_POINT ( 'NONE',  ( 3.277744210708366079, 100.0000000000000142, -23.71256836663369327 ) ) ;
#4764 = B_SPLINE_SURFACE_WITH_KNOTS ( 'NONE', 3, 1, ( 
 ( #9793, #1740 ),
 ( #7340, #918 ),
 ( #2632, #7243 ),
 ( #1786, #7195 ),
 ( #6465, #4937 ),
 ( #4111, #23 ),
 ( #6414, #3363 ),
 ( #3274, #3226 ),
 ( #8770, #9603 ),
 ( #7293, #132 ),
 ( #8135, #6556 ),
 ( #2436, #9747 ),
 ( #81, #2584 ),
 ( #6511, #5919 ),
 ( #4251, #5235 ) ),
 .UNSPECIFIED., .F., .F., .F.,
 ( 4, 1, 1, 1, 1, 1, 1, 1, 1, 1, 1, 1, 4 ),
 ( 2, 2 ),
 ( 0.000000000000000000, 0.08595325681623211533, 0.1695367914770939399, 0.2510169726856145700, 0.3324720360531058239, 0.4139176782331075444, 0.4946662699496591764, 0.5765962148649595997, 0.6610575120797289594, 0.7465372922784411225, 0.8302848992160567487, 0.9144215288650135998, 1.000000000000000000 ),
 ( 0.000000000000000000, 1.000000000000000000 ),
 .UNSPECIFIED. ) ;
#4765 = CARTESIAN_POINT ( 'NONE',  ( -22.69253165798458127, 100.0000000000000142, -10.28928739654909563 ) ) ;
#4766 = CARTESIAN_POINT ( 'NONE',  ( 2.256430356249999658, -3.478124999385482585, -1.302750673588581432 ) ) ;
#4767 = CARTESIAN_POINT ( 'NONE',  ( -21.79396932678589849, 99.50000000000000000, -9.306975108219608828 ) ) ;
#4768 = ORIENTED_EDGE ( 'NONE', *, *, #4103, .T. ) ;
#4769 = AXIS2_PLACEMENT_3D ( 'NONE', #3200, #153, #7262 ) ;
#4770 = ORIENTED_EDGE ( 'NONE', *, *, #6044, .F. ) ;
#4771 = CARTESIAN_POINT ( 'NONE',  ( 2.256430356249999658, -1.678124999385482541, -1.302750673588581432 ) ) ;
#4772 = CARTESIAN_POINT ( 'NONE',  ( -27.43301270000000969, 1.599999998907525534, 11.36312591709335429 ) ) ;
#4773 = DIRECTION ( 'NONE',  ( -0.000000000000000000, -1.000000000000000000, -0.000000000000000000 ) ) ;
#4774 = CARTESIAN_POINT ( 'NONE',  ( -27.00000000000000355, 3.550000000000000266, -11.18376618407357093 ) ) ;
#4775 = CARTESIAN_POINT ( 'NONE',  ( -20.63200021313574695, 99.50000000000000000, -10.19493994959453431 ) ) ;
#4776 = ORIENTED_EDGE ( 'NONE', *, *, #6072, .T. ) ;
#4777 = AXIS2_PLACEMENT_3D ( 'NONE', #7461, #6578, #9678 ) ;
#4778 = CARTESIAN_POINT ( 'NONE',  ( 8.467217662126737210, 100.0000000000000142, 20.02246181083229004 ) ) ;
#4779 = AXIS2_PLACEMENT_3D ( 'NONE', #5030, #6699, #9068 ) ;
#4780 = CARTESIAN_POINT ( 'NONE',  ( 4.786228327491941173E-16, -3.740624999385482319, 2.605501347177161087 ) ) ;
#4781 = ORIENTED_EDGE ( 'NONE', *, *, #2496, .F. ) ;
#4782 = CARTESIAN_POINT ( 'NONE',  ( 11.36312591709336139, 1.199999998907525178, -27.43301270000000258 ) ) ;
#4783 = CARTESIAN_POINT ( 'NONE',  ( -27.00000000000000355, 2.000000000000000000, -3.306546357697854128E-15 ) ) ;
#4784 = EDGE_CURVE ( 'NONE', #3764, #1470, #1077, .T. ) ;
#4785 = DIRECTION ( 'NONE',  ( 0.000000000000000000, 0.000000000000000000, -1.000000000000000000 ) ) ;
#4786 = CARTESIAN_POINT ( 'NONE',  ( -2.256430356250000102, -2.953124999385482674, 0.000000000000000000 ) ) ;
#4787 = DIRECTION ( 'NONE',  ( -0.000000000000000000, -1.000000000000000000, -0.000000000000000000 ) ) ;
#4788 = CARTESIAN_POINT ( 'NONE',  ( -16.87593989452418697, 99.99999999999998579, 15.58794934546231126 ) ) ;
#4789 = CARTESIAN_POINT ( 'NONE',  ( 27.00000000000000355, 5.399999997815051245, 0.000000000000000000 ) ) ;
#4790 = CARTESIAN_POINT ( 'NONE',  ( -2.499999999999999556, -2.606249998770965526, 1.443375672974065882 ) ) ;
#4791 = VECTOR ( 'NONE', #1602, 1000.000000000000114 ) ;
#4792 = CARTESIAN_POINT ( 'NONE',  ( 0.6698729810778075722, -1.161153809338631770, 2.499999999999999556 ) ) ;
#4793 = DIRECTION ( 'NONE',  ( -0.000000000000000000, 1.000000000000000000, -0.000000000000000000 ) ) ;
#4794 = CARTESIAN_POINT ( 'NONE',  ( -21.93524539549613550, 99.49999999999998579, -11.03420246938663318 ) ) ;
#4795 = CARTESIAN_POINT ( 'NONE',  ( 1.128215178124999607, -4.340624999385482852, -1.954126010382871259 ) ) ;
#4796 = ORIENTED_EDGE ( 'NONE', *, *, #6012, .F. ) ;
#4797 = VECTOR ( 'NONE', #109, 1000.000000000000000 ) ;
#4798 = VERTEX_POINT ( 'NONE', #6939 ) ;
#4799 = LINE ( 'NONE', #7996, #254 ) ;
#4800 =( REPRESENTATION_RELATIONSHIP ('NONE','NONE', #3375, #177 ) REPRESENTATION_RELATIONSHIP_WITH_TRANSFORMATION ( #3824 )SHAPE_REPRESENTATION_RELATIONSHIP( ) );
#4801 = VECTOR ( 'NONE', #7398, 1000.000000000000000 ) ;
#4802 = ORIENTED_EDGE ( 'NONE', *, *, #8074, .T. ) ;
#4803 = SURFACE_STYLE_FILL_AREA ( #672 ) ;
#4804 = CARTESIAN_POINT ( 'NONE',  ( 1.250000000000001110, -2.043749998770965970, 2.165063509461096380 ) ) ;
#4805 = EDGE_CURVE ( 'NONE', #2167, #5722, #10081, .T. ) ;
#4806 = LINE ( 'NONE', #10363, #3628 ) ;
#4807 = CARTESIAN_POINT ( 'NONE',  ( -11.36312591709335962, 4.599999998907525978, -27.43301270000000258 ) ) ;
#4808 = ADVANCED_FACE ( 'NONE', ( #4427 ), #9292, .T. ) ;
#4809 = CARTESIAN_POINT ( 'NONE',  ( 2.500000000000000000, -4.724999999999998757, -3.061616997868383141E-16 ) ) ;
#4810 = CARTESIAN_POINT ( 'NONE',  ( 2.256430356250000102, -3.178124999385482319, -2.763330213280484622E-16 ) ) ;
#4811 = CARTESIAN_POINT ( 'NONE',  ( 3.403200340195960738, 99.99999999999998579, -22.39827506699316118 ) ) ;
#4812 = CARTESIAN_POINT ( 'NONE',  ( -2.256430356249999214, -3.815624999385482941, 1.302750673588581876 ) ) ;
#4813 = FACE_OUTER_BOUND ( 'NONE', #5212, .T. ) ;
#4814 = CARTESIAN_POINT ( 'NONE',  ( 19.09188309203678102, 2.099999997815050090, 19.09188309203678813 ) ) ;
#4815 = B_SPLINE_CURVE_WITH_KNOTS ( 'NONE', 3,
 ( #4276, #2705, #5997, #7839, #1290, #4592, #6886, #9189, #7783, #10083, #2185, #6102, #2863, #4428, #5440, #2008, #9235, #8575, #3757 ),
 .UNSPECIFIED., .F., .F.,
 ( 4, 1, 1, 1, 1, 1, 1, 1, 1, 1, 1, 1, 1, 1, 1, 1, 4 ),
 ( 0.000000000000000000, 0.06358429906668214282, 0.1250797439647324816, 0.1854075229911844314, 0.2454523280917267347, 0.3052969617611028252, 0.3655926515411210831, 0.4275661794825392770, 0.4916205250740160460, 0.5555554127340263104, 0.6185525978810689773, 0.6803322039413655098, 0.7423868736098769849, 0.8044290668430417179, 0.8676072479036442964, 0.9329923078238739897, 1.000000000000000000 ),
 .UNSPECIFIED. ) ;
#4816 = CARTESIAN_POINT ( 'NONE',  ( -20.63200021313574695, 99.50000000000000000, -10.19493994959453431 ) ) ;
#4817 = CARTESIAN_POINT ( 'NONE',  ( 3.597125852879613728, 99.49999999999998579, -24.22990373345680126 ) ) ;
#4818 = CARTESIAN_POINT ( 'NONE',  ( 3.356341388373609291, 100.0000000000000142, -21.61643044175963979 ) ) ;
#4819 = DIRECTION ( 'NONE',  ( 0.9985355274883277454, 0.000000000000000000, -0.05409991075415103434 ) ) ;
#4820 = VECTOR ( 'NONE', #265, 1000.000000000000000 ) ;
#4821 = CARTESIAN_POINT ( 'NONE',  ( 2.256430356250000102, -2.615624999385482763, -2.763330213280484622E-16 ) ) ;
#4822 = CARTESIAN_POINT ( 'NONE',  ( -20.77412980915959650, 99.49999999999997158, -9.759484723497815040 ) ) ;
#4823 = ORIENTED_EDGE ( 'NONE', *, *, #2386, .F. ) ;
#4824 = CARTESIAN_POINT ( 'NONE',  ( 1.128215178125001161, -1.790624999385482807, 1.954126010382870815 ) ) ;
#4825 = CARTESIAN_POINT ( 'NONE',  ( 27.43301269999999548, 4.999999998907525445, 11.36312591709337738 ) ) ;
#4826 = CARTESIAN_POINT ( 'NONE',  ( -16.25490828497592588, 99.49999999999998579, 14.91257814242970348 ) ) ;
#4827 = CARTESIAN_POINT ( 'NONE',  ( -19.09188309203678813, 4.500000000000000888, 19.09188309203678457 ) ) ;
#4828 = VECTOR ( 'NONE', #2696, 1000.000000000000000 ) ;
#4829 = CARTESIAN_POINT ( 'NONE',  ( 2.874264611687397331, 99.50000000000001421, -22.24889838548798693 ) ) ;
#4830 = VERTEX_POINT ( 'NONE', #4373 ) ;
#4831 =( NAMED_UNIT ( * ) PLANE_ANGLE_UNIT ( ) SI_UNIT ( $, .RADIAN. ) );
#4832 = CARTESIAN_POINT ( 'NONE',  ( 11.18376618407357626, 2.049999997815050268, 27.00000000000000000 ) ) ;
#4833 = ORIENTED_EDGE ( 'NONE', *, *, #5449, .T. ) ;
#4834 = CARTESIAN_POINT ( 'NONE',  ( 4.871887406949175769, 99.49999999999995737, -23.77896509604281405 ) ) ;
#4835 = VERTEX_POINT ( 'NONE', #452 ) ;
#4836 = CARTESIAN_POINT ( 'NONE',  ( -27.43301270000000258, 3.849999998907525534, -3.359575119402369376E-15 ) ) ;
#4837 = CARTESIAN_POINT ( 'NONE',  ( 1.249999999999999334, -4.143749998770966059, -2.165063509461096825 ) ) ;
#4838 = DIRECTION ( 'NONE',  ( -0.000000000000000000, -1.000000000000000000, -0.000000000000000000 ) ) ;
#4839 = CARTESIAN_POINT ( 'NONE',  ( -2.256430356250000102, -4.340624999385482852, -1.302750673588580321 ) ) ;
#4840 = PLANE ( 'NONE',  #5882 ) ;
#4841 = CARTESIAN_POINT ( 'NONE',  ( 19.09188309203678813, 1.700000000000000178, -19.09188309203678813 ) ) ;
#4842 = CARTESIAN_POINT ( 'NONE',  ( 8.540544597724410991, 100.0000000000000000, 19.98924338346217766 ) ) ;
#4843 = ORIENTED_EDGE ( 'NONE', *, *, #2909, .T. ) ;
#4844 = EDGE_CURVE ( 'NONE', #9400, #8029, #2810, .T. ) ;
#4845 = CARTESIAN_POINT ( 'NONE',  ( 2.500000000000000000, -1.931249998770965481, -1.443375672974064994 ) ) ;
#4846 = ORIENTED_EDGE ( 'NONE', *, *, #5943, .T. ) ;
#4847 = CARTESIAN_POINT ( 'NONE',  ( 4.358720771404392735, 100.0000000000000000, -21.20742720589606378 ) ) ;
#4848 = CARTESIAN_POINT ( 'NONE',  ( -15.72775836928289017, 99.50000000000000000, 17.03252426573849476 ) ) ;
#4849 = CARTESIAN_POINT ( 'NONE',  ( 9.778118981323553172, 99.49999999999998579, 20.11889122584574352 ) ) ;
#4850 = CARTESIAN_POINT ( 'NONE',  ( 2.256430356250000546, -3.553124999385482763, 1.302750673588579877 ) ) ;
#4851 = B_SPLINE_SURFACE_WITH_KNOTS ( 'NONE', 3, 1, ( 
 ( #3268, #1645 ),
 ( #9599, #6461 ),
 ( #3360, #2535 ),
 ( #4932, #7979 ),
 ( #6359, #4888 ),
 ( #2430, #8131 ),
 ( #5678, #3175 ),
 ( #8084, #1692 ),
 ( #9553, #6409 ),
 ( #9506, #913 ),
 ( #7138, #4105 ),
 ( #7289, #129 ),
 ( #3316, #4153 ),
 ( #7336, #2331 ),
 ( #5528, #8721 ),
 ( #1539, #812 ),
 ( #4734, #10343 ),
 ( #4006, #7190 ),
 ( #19, #5626 ) ),
 .UNSPECIFIED., .F., .F., .F.,
 ( 4, 1, 1, 1, 1, 1, 1, 1, 1, 1, 1, 1, 1, 1, 1, 1, 4 ),
 ( 2, 2 ),
 ( 0.000000000000000000, 0.08029080299619884009, 0.1602734547033792534, 0.2412010114815648643, 0.3246404098231062685, 0.3670482715230247162, 0.4085690013065461645, 0.4496707568484641926, 0.4905395156191099670, 0.5313644394553277417, 0.5726744073239632415, 0.6138178896263115636, 0.6555018086025313773, 0.7394546411270094266, 0.8240219501092651555, 0.9101625766452680066, 1.000000000000000000 ),
 ( 0.000000000000000000, 1.000000000000000000 ),
 .UNSPECIFIED. ) ;
#4852 = ORIENTED_EDGE ( 'NONE', *, *, #4686, .F. ) ;
#4853 = DIRECTION ( 'NONE',  ( 0.000000000000000000, -0.000000000000000000, 1.000000000000000000 ) ) ;
#4854 = ADVANCED_FACE ( 'NONE', ( #6099 ), #10293, .T. ) ;
#4855 = FILL_AREA_STYLE_COLOUR ( '', #9028 ) ;
#4856 =( BOUNDED_CURVE ( )  B_SPLINE_CURVE ( 2, ( #7443, #6570, #5784, #8193, #5090, #4214, #5743, #3287, #5039 ),
 .UNSPECIFIED., .F., .T. ) 
 B_SPLINE_CURVE_WITH_KNOTS ( ( 3, 2, 2, 2, 3 ),
 ( 0.2708333333333333703, 0.2777777777777777901, 0.2916666666666666852, 0.3055555555555555802, 0.3125000000000000000 ),
 .UNSPECIFIED. ) 
 CURVE ( )  GEOMETRIC_REPRESENTATION_ITEM ( )  RATIONAL_B_SPLINE_CURVE ( ( 0.9330127018922194093, 0.9330127018922196314, 1.000000000000000000, 0.8660254037844387076, 1.000000000000000000, 0.8660254037844387076, 1.000000000000000000, 0.9330127018922194093, 0.9330127018922194093 ) ) 
 REPRESENTATION_ITEM ( '' )  );
#4857 = CARTESIAN_POINT ( 'NONE',  ( -0.6698729810778105698, -3.507596189432333311, 2.499999999999997780 ) ) ;
#4858 = CARTESIAN_POINT ( 'NONE',  ( 11.18376618407357093, 3.149999997815050801, -27.00000000000000355 ) ) ;
#4859 = CARTESIAN_POINT ( 'NONE',  ( 8.901217755223779449, 100.0000000000000426, 19.92336871027421097 ) ) ;
#4860 = ORIENTED_EDGE ( 'NONE', *, *, #7145, .F. ) ;
#4861 = ADVANCED_FACE ( 'NONE', ( #4738 ), #2334, .T. ) ;
#4862 =( NAMED_UNIT ( * ) PLANE_ANGLE_UNIT ( ) SI_UNIT ( $, .RADIAN. ) );
#4863 = CARTESIAN_POINT ( 'NONE',  ( 3.282077632710153292, 99.50000000000000000, -23.74569985055724786 ) ) ;
#4864 = CARTESIAN_POINT ( 'NONE',  ( 1.128215178125001161, -5.053124999385482319, 1.954126010382870815 ) ) ;
#4865 = ADVANCED_FACE ( 'NONE', ( #8724 ), #4689, .T. ) ;
#4866 = CARTESIAN_POINT ( 'NONE',  ( -20.70854316912038229, 99.50000000000001421, -10.95957977981033515 ) ) ;
#4867 = CARTESIAN_POINT ( 'NONE',  ( 19.09188309203678813, 2.299999997815050712, -19.09188309203678813 ) ) ;
#4868 = CARTESIAN_POINT ( 'NONE',  ( 0.6698729810778050187, -2.117403810567665801, 2.500000000000000444 ) ) ;
#4869 = EDGE_CURVE ( 'NONE', #1454, #1485, #1436, .T. ) ;
#4870 = DIRECTION ( 'NONE',  ( 1.000000000000000000, 0.000000000000000000, 0.000000000000000000 ) ) ;
#4871 = FACE_OUTER_BOUND ( 'NONE', #409, .T. ) ;
#4872 = DIRECTION ( 'NONE',  ( 0.9961946980917455452, -0.08715574274765837404, 0.000000000000000000 ) ) ;
#4873 = CARTESIAN_POINT ( 'NONE',  ( -2.256430356250000102, -3.290624999385482585, 0.000000000000000000 ) ) ;
#4874 = CARTESIAN_POINT ( 'NONE',  ( 9.526533506306627430, 100.0000000000000000, 21.03094362668609207 ) ) ;
#4875 = ORIENTED_EDGE ( 'NONE', *, *, #2754, .F. ) ;
#4876 = CARTESIAN_POINT ( 'NONE',  ( -2.256430356250000102, -4.678124999385483207, -1.302750673588580321 ) ) ;
#4877 = CARTESIAN_POINT ( 'NONE',  ( 11.36312591709336139, 2.099999998907525089, -27.43301270000000258 ) ) ;
#4878 = DIRECTION ( 'NONE',  ( 0.000000000000000000, -1.000000000000000000, 0.000000000000000000 ) ) ;
#4879 = CARTESIAN_POINT ( 'NONE',  ( -4.959819536546781389E-15, 3.799999999999999822, 27.00000000000000355 ) ) ;
#4880 = CARTESIAN_POINT ( 'NONE',  ( -21.16695614262292580, 100.0000000000000000, -11.33496398805607441 ) ) ;
#4881 = VECTOR ( 'NONE', #6695, 1000.000000000000000 ) ;
#4882 = VERTEX_POINT ( 'NONE', #6604 ) ;
#4883 = ADVANCED_FACE ( 'NONE', ( #4059 ), #4764, .T. ) ;
#4884 = DIRECTION ( 'NONE',  ( -0.000000000000000000, 1.000000000000000000, -0.000000000000000000 ) ) ;
#4885 = CARTESIAN_POINT ( 'NONE',  ( -21.03403678956047074, 99.50000000000001421, -10.80451401317004922 ) ) ;
#4886 = CARTESIAN_POINT ( 'NONE',  ( -20.72805389903318130, 99.50000000000000000, -9.848585782927868237 ) ) ;
#4887 = CARTESIAN_POINT ( 'NONE',  ( -11.36312591709337561, 3.199999998907525178, 27.43301269999999548 ) ) ;
#4888 = CARTESIAN_POINT ( 'NONE',  ( 3.097283534322414766, 100.0000000000000284, -24.18405864774921454 ) ) ;
#4889 = VECTOR ( 'NONE', #5629, 1000.000000000000000 ) ;
#4890 = DIRECTION ( 'NONE',  ( -0.05422338932609765960, 0.000000000000000000, -0.9985288298541962204 ) ) ;
#4891 = CARTESIAN_POINT ( 'NONE',  ( -1.128215178124998497, -4.678124999385482319, 1.954126010382872147 ) ) ;
#4892 = CARTESIAN_POINT ( 'NONE',  ( -16.40919047799676989, 100.0000000000000000, 16.38364531277195013 ) ) ;
#4893 = CARTESIAN_POINT ( 'NONE',  ( -16.67860655220511035, 99.49999999999998579, 15.23428378554110374 ) ) ;
#4894 = CARTESIAN_POINT ( 'NONE',  ( 8.467217662126737210, 100.0000000000000142, 20.02246181083229004 ) ) ;
#4895 = VECTOR ( 'NONE', #8027, 1000.000000000000000 ) ;
#4896 = CARTESIAN_POINT ( 'NONE',  ( -2.499999999999999556, -4.406249998770965348, 1.443375672974065882 ) ) ;
#4897 = VERTEX_POINT ( 'NONE', #1107 ) ;
#4898 = CARTESIAN_POINT ( 'NONE',  ( -22.28244091826395135, 99.99999999999997158, -10.68852969318427881 ) ) ;
#4899 = CARTESIAN_POINT ( 'NONE',  ( 1.034219503716432668E-14, -3.262500000000000178, -2.500000000000000000 ) ) ;
#4900 = EDGE_CURVE ( 'NONE', #7872, #6035, #8331, .T. ) ;
#4901 = CARTESIAN_POINT ( 'NONE',  ( -21.58460863908062066, 99.50000000000002842, -11.10356610083683648 ) ) ;
#4902 = CARTESIAN_POINT ( 'NONE',  ( -2.256430356249999214, -3.253124999385482941, 1.302750673588581876 ) ) ;
#4903 = VECTOR ( 'NONE', #1179, 999.9999999999998863 ) ;
#4904 = CARTESIAN_POINT ( 'NONE',  ( 8.091962505948220752, 99.49999999999995737, 20.48385654212622242 ) ) ;
#4905 = CARTESIAN_POINT ( 'NONE',  ( 0.000000000000000000, 0.000000000000000000, -2.500000000000000000 ) ) ;
#4906 = CARTESIAN_POINT ( 'NONE',  ( -16.12578516900833137, 100.0000000000000142, 15.23469143358620492 ) ) ;
#4907 = CARTESIAN_POINT ( 'NONE',  ( -19.09188309203678457, 4.299999999999999822, -19.09188309203678813 ) ) ;
#4908 = ORIENTED_EDGE ( 'NONE', *, *, #9899, .F. ) ;
#4909 = EDGE_CURVE ( 'NONE', #2567, #6863, #2840, .T. ) ;
#4910 = CARTESIAN_POINT ( 'NONE',  ( -21.30928386698190025, 100.0000000000000000, -11.02857376369709996 ) ) ;
#4911 = CARTESIAN_POINT ( 'NONE',  ( 1.128215178124999607, -0.2906249993854829738, -1.954126010382871259 ) ) ;
#4912 = CARTESIAN_POINT ( 'NONE',  ( 3.986298408513477387, 100.0000000000000568, -22.53092616755505162 ) ) ;
#4913 = CARTESIAN_POINT ( 'NONE',  ( -27.00000000000000355, 0.9999999978150503344, -3.306546357697854128E-15 ) ) ;
#4914 =( BOUNDED_CURVE ( )  B_SPLINE_CURVE ( 2, ( #1711, #4126, #4907, #8102, #3335, #933, #148, #5286, #3672 ),
 .UNSPECIFIED., .F., .F. ) 
 B_SPLINE_CURVE_WITH_KNOTS ( ( 3, 2, 2, 2, 3 ),
 ( 0.7500000000000000000, 0.7678571428571429047, 0.7857142857142856984, 0.8035714285714286031, 0.8214285714285713969 ),
 .UNSPECIFIED. ) 
 CURVE ( )  GEOMETRIC_REPRESENTATION_ITEM ( )  RATIONAL_B_SPLINE_CURVE ( ( 1.000000000000000000, 0.9238795325112867385, 1.000000000000000000, 0.9238795325112867385, 1.000000000000000000, 0.9238795325112867385, 1.000000000000000000, 0.9238795325112867385, 1.000000000000000000 ) ) 
 REPRESENTATION_ITEM ( '' )  );
#4915 = CARTESIAN_POINT ( 'NONE',  ( 3.296462644833695776, 99.50000000000001421, -23.81854410834942115 ) ) ;
#4916 = CARTESIAN_POINT ( 'NONE',  ( 3.198592217420132666, 100.0000000000000000, -21.96964977087737836 ) ) ;
#4917 = DIRECTION ( 'NONE',  ( 0.000000000000000000, 3.537534599156363020E-12, -1.000000000000000000 ) ) ;
#4918 = CARTESIAN_POINT ( 'NONE',  ( 2.256430356249999658, -4.378124999385483385, -1.302750673588581432 ) ) ;
#4919 = ORIENTED_EDGE ( 'NONE', *, *, #3469, .F. ) ;
#4920 = EDGE_LOOP ( 'NONE', ( #4875, #6855, #543, #7414 ) ) ;
#4921 = CARTESIAN_POINT ( 'NONE',  ( -2.256430356250000102, -5.090624999385482852, 0.000000000000000000 ) ) ;
#4922 = CARTESIAN_POINT ( 'NONE',  ( -15.07178375341841381, 99.50000000000000000, 16.66969090848992607 ) ) ;
#4923 = CARTESIAN_POINT ( 'NONE',  ( -27.43301270000000258, 0.5999999989075250895, -11.36312591709336317 ) ) ;
#4924 = CARTESIAN_POINT ( 'NONE',  ( 0.000000000000000000, 100.0000000000000000, 0.000000000000000000 ) ) ;
#4925 = VECTOR ( 'NONE', #6349, 1000.000000000000000 ) ;
#4926 = CARTESIAN_POINT ( 'NONE',  ( -16.35834224700816009, 99.99999999999995737, 16.43761959438736397 ) ) ;
#4927 = CARTESIAN_POINT ( 'NONE',  ( 19.09188309203678813, 2.299999997815050712, -19.09188309203678813 ) ) ;
#4928 = ORIENTED_EDGE ( 'NONE', *, *, #4537, .F. ) ;
#4929 = EDGE_CURVE ( 'NONE', #2398, #6279, #9014, .T. ) ;
#4930 = DIRECTION ( 'NONE',  ( 0.000000000000000000, 0.000000000000000000, -1.000000000000000000 ) ) ;
#4931 = VECTOR ( 'NONE', #5712, 1000.000000000000000 ) ;
#4932 = CARTESIAN_POINT ( 'NONE',  ( 3.024867170474271116, 99.49999999999995737, -24.05477125543085748 ) ) ;
#4933 = ADVANCED_FACE ( 'NONE', ( #9167 ), #6926, .T. ) ;
#4934 = FILL_AREA_STYLE_COLOUR ( '', #2728 ) ;
#4935 = CARTESIAN_POINT ( 'NONE',  ( -1.128215178124998497, -4.228124999385482141, 1.954126010382872147 ) ) ;
#4936 = DIRECTION ( 'NONE',  ( -0.000000000000000000, -1.000000000000000000, -0.000000000000000000 ) ) ;
#4937 = CARTESIAN_POINT ( 'NONE',  ( -22.43208371148383762, 100.0000000000000000, -9.654966607469265938 ) ) ;
#4938 = CARTESIAN_POINT ( 'NONE',  ( 8.231219904624582639, 100.0000000000000000, 20.21381436664452735 ) ) ;
#4939 = CARTESIAN_POINT ( 'NONE',  ( -1.249999999999998224, -5.268749998770966059, 2.165063509461097713 ) ) ;
#4940 = ORIENTED_EDGE ( 'NONE', *, *, #143, .T. ) ;
#4941 = DIRECTION ( 'NONE',  ( -0.000000000000000000, -1.000000000000000000, -0.000000000000000000 ) ) ;
#4942 = CARTESIAN_POINT ( 'NONE',  ( 3.552835461024879127, 99.99999999999997158, -21.47801279722421697 ) ) ;
#4943 = CARTESIAN_POINT ( 'NONE',  ( -14.89910828679519739, 99.99999999999997158, 16.44921749203638939 ) ) ;
#4944 = CARTESIAN_POINT ( 'NONE',  ( -1.128215178125000273, -2.915624999385482585, -1.954126010382871259 ) ) ;
#4945 = ORIENTED_EDGE ( 'NONE', *, *, #2183, .T. ) ;
#4946 = CARTESIAN_POINT ( 'NONE',  ( 8.064245308217579122, 99.49999999999998579, 20.64099956338070641 ) ) ;
#4947 = VECTOR ( 'NONE', #10168, 1000.000000000000000 ) ;
#4948 = DIRECTION ( 'NONE',  ( 0.000000000000000000, 0.000000000000000000, -1.000000000000000000 ) ) ;
#4949 = CARTESIAN_POINT ( 'NONE',  ( -22.28244091826395135, 100.0000000000000000, -10.68852969318427881 ) ) ;
#4950 = CARTESIAN_POINT ( 'NONE',  ( 4.320351800798612807, 99.49999999999995737, -21.62386382141117736 ) ) ;
#4951 = AXIS2_PLACEMENT_3D ( 'NONE', #7719, #5987, #4583 ) ;
#4952 = VECTOR ( 'NONE', #1800, 1000.000000000000000 ) ;
#4953 = CARTESIAN_POINT ( 'NONE',  ( 3.977571997893210032, 99.50000000000000000, -24.70179182097838932 ) ) ;
#4954 = CARTESIAN_POINT ( 'NONE',  ( 4.232447118646125439, 99.99999999999995737, -21.54138831197867887 ) ) ;
#4955 = FACE_OUTER_BOUND ( 'NONE', #2093, .T. ) ;
#4956 = CARTESIAN_POINT ( 'NONE',  ( 27.00000000000000355, 4.649999997815049468, -11.18376618407356737 ) ) ;
#4957 = CARTESIAN_POINT ( 'NONE',  ( 0.000000000000000000, 0.000000000000000000, 0.000000000000000000 ) ) ;
#4958 = CARTESIAN_POINT ( 'NONE',  ( 2.500000000000000444, -4.706249998770965171, 1.443375672974063439 ) ) ;
#4959 = LINE ( 'NONE', #4181, #6239 ) ;
#4960 = EDGE_CURVE ( 'NONE', #6136, #8554, #5776, .T. ) ;
#4961 = CARTESIAN_POINT ( 'NONE',  ( -7.500000000000000888, 104.5000000000000142, 3.000000000000000000 ) ) ;
#4962 = CARTESIAN_POINT ( 'NONE',  ( 1.034219503716432668E-14, -5.006249998770964993, -2.500000000000000000 ) ) ;
#4963 = CARTESIAN_POINT ( 'NONE',  ( -1.728534191064767578, -5.141148192311419507, -1.450395636689028711 ) ) ;
#4964 = SURFACE_STYLE_FILL_AREA ( #3350 ) ;
#4965 = CARTESIAN_POINT ( 'NONE',  ( 7.156925775808251622, 99.50000000000000000, 23.91622092442889524 ) ) ;
#4966 =( BOUNDED_CURVE ( )  B_SPLINE_CURVE ( 2, ( #7516, #206, #9933, #3547, #8207, #6735, #253, #5163, #8996 ),
 .UNSPECIFIED., .F., .F. ) 
 B_SPLINE_CURVE_WITH_KNOTS ( ( 3, 2, 2, 2, 3 ),
 ( 0.3958333333333333703, 0.4027777777777777901, 0.4166666666666666852, 0.4305555555555555802, 0.4375000000000000000 ),
 .UNSPECIFIED. ) 
 CURVE ( )  GEOMETRIC_REPRESENTATION_ITEM ( )  RATIONAL_B_SPLINE_CURVE ( ( 0.9330127018922194093, 0.9330127018922196314, 1.000000000000000000, 0.8660254037844387076, 1.000000000000000000, 0.8660254037844387076, 1.000000000000000000, 0.9330127018922194093, 0.9330127018922194093 ) ) 
 REPRESENTATION_ITEM ( '' )  );
#4967 = CYLINDRICAL_SURFACE ( 'NONE', #9724, 30.00000000000000000 ) ;
#4968 = CARTESIAN_POINT ( 'NONE',  ( -11.18376618407358336, 3.750000000000000000, 26.99999999999999645 ) ) ;
#4969 = CARTESIAN_POINT ( 'NONE',  ( 3.105863891863242632, 100.0000000000000142, -22.59672720503480292 ) ) ;
#4970 = CARTESIAN_POINT ( 'NONE',  ( -2.500000000000000000, -1.349999999999999867, 0.000000000000000000 ) ) ;
#4971 = DIRECTION ( 'NONE',  ( 0.000000000000000000, -0.000000000000000000, 1.000000000000000000 ) ) ;
#4972 = CARTESIAN_POINT ( 'NONE',  ( -20.95611194834973645, 99.99999999999997158, -10.07788454426966318 ) ) ;
#4973 = EDGE_CURVE ( 'NONE', #2426, #2647, #9107, .T. ) ;
#4974 = ORIENTED_EDGE ( 'NONE', *, *, #4419, .T. ) ;
#4975 = CARTESIAN_POINT ( 'NONE',  ( -21.59614764830937972, 99.50000000000001421, -9.292069227195950631 ) ) ;
#4976 = CARTESIAN_POINT ( 'NONE',  ( 2.500000000000000444, -1.556249998770966148, 1.443375672974063439 ) ) ;
#4977 = CARTESIAN_POINT ( 'NONE',  ( -15.56095293356939813, 99.50000000000001421, 15.23332223661997453 ) ) ;
#4978 = CARTESIAN_POINT ( 'NONE',  ( -21.16695614262292580, 100.0000000000000000, -11.33496398805607441 ) ) ;
#4979 = AXIS2_PLACEMENT_3D ( 'NONE', #10072, #9347, #8395 ) ;
#4980 = CARTESIAN_POINT ( 'NONE',  ( 2.256430356250000102, -3.628124999385482496, -2.763330213280484622E-16 ) ) ;
#4981 = CARTESIAN_POINT ( 'NONE',  ( -22.69253165798458127, 99.50000000000001421, -10.28928739654909563 ) ) ;
#4982 = CARTESIAN_POINT ( 'NONE',  ( -16.88522588321459494, 100.0000000000000284, 16.18266969485829421 ) ) ;
#4983 = CARTESIAN_POINT ( 'NONE',  ( 4.599186066243659887, 100.0000000000000284, -24.59301055568561623 ) ) ;
#4984 = EDGE_CURVE ( 'NONE', #7488, #7789, #2168, .T. ) ;
#4985 = CARTESIAN_POINT ( 'NONE',  ( -1.249999999999998224, -3.918749998770965082, 2.165063509461097713 ) ) ;
#4986 = VERTEX_POINT ( 'NONE', #4677 ) ;
#4987 = VERTEX_POINT ( 'NONE', #5360 ) ;
#4988 = DIRECTION ( 'NONE',  ( 0.000000000000000000, -1.000000000000000000, 0.000000000000000000 ) ) ;
#4989 = DIRECTION ( 'NONE',  ( 0.000000000000000000, -0.000000000000000000, -1.000000000000000000 ) ) ;
#4990 = EDGE_CURVE ( 'NONE', #2804, #358, #1530, .T. ) ;
#4991 = CARTESIAN_POINT ( 'NONE',  ( 9.600410285814406919, 99.49999999999998579, 19.87914582625927196 ) ) ;
#4992 = CARTESIAN_POINT ( 'NONE',  ( 23.82500000000000284, 2.917720998968569322E-15, 0.000000000000000000 ) ) ;
#4993 = DIRECTION ( 'NONE',  ( 1.320207234900709352E-11, 1.000000000000000000, 2.368819407112974206E-12 ) ) ;
#4994 = CARTESIAN_POINT ( 'NONE',  ( -3.486133158594716510E-16, -3.712499999999999467, -2.500000000000000000 ) ) ;
#4995 = LINE ( 'NONE', #287, #1115 ) ;
#4996 = ORIENTED_EDGE ( 'NONE', *, *, #8566, .T. ) ;
#4997 = CYLINDRICAL_SURFACE ( 'NONE', #5416, 2.500000000000000000 ) ;
#4998 = CARTESIAN_POINT ( 'NONE',  ( 3.689266881520847807, 99.50000000000000000, -22.97735580002706968 ) ) ;
#4999 = CARTESIAN_POINT ( 'NONE',  ( 3.949943451936506644, 99.50000000000000000, -21.41482314084395711 ) ) ;
#5000 = ORIENTED_EDGE ( 'NONE', *, *, #5457, .F. ) ;
#5001 = CARTESIAN_POINT ( 'NONE',  ( 3.403200340195960738, 100.0000000000000142, -22.39827506699316118 ) ) ;
#5002 = CARTESIAN_POINT ( 'NONE',  ( 19.09188309203678102, 2.899999997815050357, 19.09188309203678813 ) ) ;
#5003 = CARTESIAN_POINT ( 'NONE',  ( -21.13504512532655610, 99.50000000000000000, -11.31853095674525100 ) ) ;
#5004 = CARTESIAN_POINT ( 'NONE',  ( -21.04016555629948826, 100.0000000000000142, -9.929603401003973318 ) ) ;
#5005 = DIRECTION ( 'NONE',  ( 0.000000000000000000, 0.000000000000000000, -1.000000000000000000 ) ) ;
#5006 = CARTESIAN_POINT ( 'NONE',  ( -21.65488089977124275, 99.49999999999997158, -11.10326233039539723 ) ) ;
#5007 = DIRECTION ( 'NONE',  ( 0.000000000000000000, 0.000000000000000000, -1.000000000000000000 ) ) ;
#5008 = CARTESIAN_POINT ( 'NONE',  ( 1.128215178125001161, -4.940624999385482496, 1.954126010382870815 ) ) ;
#5009 = ORIENTED_EDGE ( 'NONE', *, *, #10100, .F. ) ;
#5010 = VECTOR ( 'NONE', #1721, 999.9999999999998863 ) ;
#5011 = ORIENTED_EDGE ( 'NONE', *, *, #9313, .T. ) ;
#5012 = CARTESIAN_POINT ( 'NONE',  ( 1.128215178124999607, -3.890624999385482674, -1.954126010382871259 ) ) ;
#5013 =( LENGTH_UNIT ( ) NAMED_UNIT ( * ) SI_UNIT ( .MILLI., .METRE. ) );
#5014 = CARTESIAN_POINT ( 'NONE',  ( -15.07178375341841381, 99.99999999999998579, 15.16157792772069790 ) ) ;
#5015 = CARTESIAN_POINT ( 'NONE',  ( 9.820792995160308791, 99.50000000000000000, 20.21220011423140761 ) ) ;
#5016 = ADVANCED_FACE ( 'NONE', ( #10283 ), #3565, .F. ) ;
#5017 = CARTESIAN_POINT ( 'NONE',  ( 27.43301270000000258, 4.299999998907525267, -11.36312591709336139 ) ) ;
#5018 = CARTESIAN_POINT ( 'NONE',  ( 27.43301270000000258, 0.3499999989075252005, 0.000000000000000000 ) ) ;
#5019 = CARTESIAN_POINT ( 'NONE',  ( -0.6698729810778043525, -1.442403810567665756, -2.500000000000001332 ) ) ;
#5020 = DIRECTION ( 'NONE',  ( -0.8547548816071318667, 0.000000000000000000, 0.5190318799156541374 ) ) ;
#5021 = CARTESIAN_POINT ( 'NONE',  ( 26.99999999999999645, 2.149999997815051245, 11.18376618407358691 ) ) ;
#5022 = EDGE_LOOP ( 'NONE', ( #1749, #6205, #6376, #3809, #9862 ) ) ;
#5023 = CARTESIAN_POINT ( 'NONE',  ( 7.809833820264425519, 99.49999999999995737, 20.29999375863051370 ) ) ;
#5024 = CARTESIAN_POINT ( 'NONE',  ( 3.701176614148623756, 100.0000000000000000, -24.64875008328975170 ) ) ;
#5025 = CARTESIAN_POINT ( 'NONE',  ( -15.32348647777738826, 99.50000000000000000, 15.39505148541300450 ) ) ;
#5026 = CARTESIAN_POINT ( 'NONE',  ( -16.12311789350856017, 99.50000000000000000, 14.86696503675854686 ) ) ;
#5027 = CARTESIAN_POINT ( 'NONE',  ( 0.6698729810778050187, -2.511153809338630971, 2.500000000000000444 ) ) ;
#5028 = EDGE_CURVE ( 'NONE', #9655, #7619, #5278, .T. ) ;
#5029 = CARTESIAN_POINT ( 'NONE',  ( 9.575551604960836016, 99.50000000000001421, 20.57049984249936969 ) ) ;
#5030 = CARTESIAN_POINT ( 'NONE',  ( 27.43301270000000258, 0.2999999989075251561, 0.000000000000000000 ) ) ;
#5031 = ORIENTED_EDGE ( 'NONE', *, *, #1028, .T. ) ;
#5032 = CARTESIAN_POINT ( 'NONE',  ( 2.256430356250000102, -0.4781249993854829183, -2.763330213280484622E-16 ) ) ;
#5033 = EDGE_LOOP ( 'NONE', ( #698, #8540, #2062, #9445, #2288, #2533, #5548, #4021, #6607, #3062, #5828, #4781 ) ) ;
#5034 = CARTESIAN_POINT ( 'NONE',  ( -22.10910773081910818, 100.0000000000000142, -11.33820747227609793 ) ) ;
#5035 = CARTESIAN_POINT ( 'NONE',  ( 3.497829868842083023, 99.99999999999997158, -21.50512556757917793 ) ) ;
#5036 = DIRECTION ( 'NONE',  ( -0.1697592580069431922, 0.000000000000000000, 0.9854855627156250408 ) ) ;
#5037 = CARTESIAN_POINT ( 'NONE',  ( -21.30928386698190025, 99.50000000000000000, -11.02857376369709996 ) ) ;
#5038 = AXIS2_PLACEMENT_3D ( 'NONE', #7984, #4936, #1649 ) ;
#5039 = CARTESIAN_POINT ( 'NONE',  ( 9.877377282685029372E-16, -1.687499999999999778, 2.500000000000000000 ) ) ;
#5040 = DIRECTION ( 'NONE',  ( 0.000000000000000000, -1.000000000000000000, 0.000000000000000000 ) ) ;
#5041 = LINE ( 'NONE', #7446, #279 ) ;
#5042 = CARTESIAN_POINT ( 'NONE',  ( -3.486133158594716510E-16, -2.362499999999999378, -2.500000000000000000 ) ) ;
#5043 = MECHANICAL_DESIGN_GEOMETRIC_PRESENTATION_REPRESENTATION (  '', ( #9740 ), #4219 ) ;
#5044 = EDGE_LOOP ( 'NONE', ( #9148, #2222, #7965, #8556 ) ) ;
#5045 = CARTESIAN_POINT ( 'NONE',  ( -15.31787750341841559, 99.50000000000000000, 16.43551622900274722 ) ) ;
#5046 = CARTESIAN_POINT ( 'NONE',  ( 11.36312591709336139, 1.299999998907525267, -27.43301270000000258 ) ) ;
#5047 = LINE ( 'NONE', #8249, #1548 ) ;
#5048 = EDGE_CURVE ( 'NONE', #9797, #358, #6766, .T. ) ;
#5049 = DIRECTION ( 'NONE',  ( 0.000000000000000000, -1.000000000000000000, 0.000000000000000000 ) ) ;
#5050 = CARTESIAN_POINT ( 'NONE',  ( 4.187832255138415505, 99.50000000000001421, -21.50835573230103037 ) ) ;
#5051 = ORIENTED_EDGE ( 'NONE', *, *, #5633, .F. ) ;
#5052 = CARTESIAN_POINT ( 'NONE',  ( 9.897596448871711416, 99.49999999999998579, 20.85734708541456328 ) ) ;
#5053 = CARTESIAN_POINT ( 'NONE',  ( 27.00000000000000355, 5.449999997815051067, -11.18376618407356737 ) ) ;
#5054 = PLANE ( 'NONE',  #6852 ) ;
#5055 = AXIS2_PLACEMENT_3D ( 'NONE', #9842, #4154, #9744 ) ;
#5056 = FACE_OUTER_BOUND ( 'NONE', #6539, .T. ) ;
#5057 = DIRECTION ( 'NONE',  ( -0.9567206510497618943, 0.000000000000000000, 0.2910078965507976179 ) ) ;
#5058 = CARTESIAN_POINT ( 'NONE',  ( 3.638175769014108774, 99.99999999999998579, -21.10017783766535970 ) ) ;
#5059 = CARTESIAN_POINT ( 'NONE',  ( -0.6698729810778020211, -4.986153809338630616, -2.500000000000002665 ) ) ;
#5060 = ORIENTED_EDGE ( 'NONE', *, *, #9459, .T. ) ;
#5061 = CARTESIAN_POINT ( 'NONE',  ( -1.128215178125000273, -4.715624999385481964, -1.954126010382871259 ) ) ;
#5062 = SHAPE_REPRESENTATION_RELATIONSHIP ( 'NONE' , 'NONE' ,  #9736, #5870 ) ;
#5063 = CARTESIAN_POINT ( 'NONE',  ( -15.10737684033046335, 99.50000000000000000, 15.12848924955281049 ) ) ;
#5064 = CARTESIAN_POINT ( 'NONE',  ( 2.928963527206765338, 99.49999999999997158, -23.52685633767685758 ) ) ;
#5065 = CARTESIAN_POINT ( 'NONE',  ( -19.39806930854667755, 1.349999998907525534, -19.39806930854668110 ) ) ;
#5066 = DIRECTION ( 'NONE',  ( -0.2907782774943305504, 0.000000000000000000, -0.9567904646982169359 ) ) ;
#5067 = FACE_OUTER_BOUND ( 'NONE', #9059, .T. ) ;
#5068 = DIRECTION ( 'NONE',  ( 0.000000000000000000, 0.000000000000000000, 1.000000000000000000 ) ) ;
#5069 = PRESENTATION_STYLE_ASSIGNMENT (( #8425 ) ) ;
#5070 = ORIENTED_EDGE ( 'NONE', *, *, #2658, .T. ) ;
#5071 = CARTESIAN_POINT ( 'NONE',  ( 7.771508748547515388, 99.50000000000001421, 20.40818475981234315 ) ) ;
#5072 = CARTESIAN_POINT ( 'NONE',  ( 2.500000000000000000, -1.481249998770965970, -1.443375672974065438 ) ) ;
#5073 = CARTESIAN_POINT ( 'NONE',  ( 9.526533506306627430, 99.50000000000000000, 21.03094362668609207 ) ) ;
#5074 = CARTESIAN_POINT ( 'NONE',  ( 27.00000000000000355, 4.800000000000000711, 0.000000000000000000 ) ) ;
#5075 = AXIS2_PLACEMENT_3D ( 'NONE', #8330, #9952, #2629 ) ;
#5076 = CARTESIAN_POINT ( 'NONE',  ( -16.36470918167357169, 100.0000000000000000, 16.79054296464299867 ) ) ;
#5077 = CARTESIAN_POINT ( 'NONE',  ( 9.547662139763570366, 99.99999999999991473, 20.94662037603165672 ) ) ;
#5078 = CARTESIAN_POINT ( 'NONE',  ( -15.07178375341841559, 99.50000000000001421, 15.16157792772069968 ) ) ;
#5079 = ORIENTED_EDGE ( 'NONE', *, *, #7948, .F. ) ;
#5080 = CARTESIAN_POINT ( 'NONE',  ( -16.24524625128438515, 100.0000000000000284, 16.53274063862002308 ) ) ;
#5081 = CARTESIAN_POINT ( 'NONE',  ( 1.250000000000001110, -4.293749998770965526, 2.165063509461096380 ) ) ;
#5082 = ORIENTED_EDGE ( 'NONE', *, *, #4784, .F. ) ;
#5083 = EDGE_CURVE ( 'NONE', #5876, #2748, #6416, .T. ) ;
#5084 = CARTESIAN_POINT ( 'NONE',  ( -22.35642768247353729, 99.49999999999995737, -10.34293228154892752 ) ) ;
#5085 = CARTESIAN_POINT ( 'NONE',  ( 0.000000000000000000, 0.000000000000000000, 0.000000000000000000 ) ) ;
#5086 = AXIS2_PLACEMENT_3D ( 'NONE', #7612, #507, #8459 ) ;
#5087 = DIRECTION ( 'NONE',  ( -0.8660254037844387076, -0.000000000000000000, 0.4999999999999997780 ) ) ;
#5088 = CARTESIAN_POINT ( 'NONE',  ( 0.000000000000000000, -25.00000000000000000, 0.000000000000000000 ) ) ;
#5089 = B_SPLINE_CURVE_WITH_KNOTS ( 'NONE', 3,
 ( #5986, #8506, #2176, #390, #1391, #3746, #5375, #2908, #441, #8564, #6093, #10017, #4364, #2970, #9227, #9285, #1336, #1281, #2118 ),
 .UNSPECIFIED., .F., .F.,
 ( 4, 1, 1, 1, 1, 1, 1, 1, 1, 1, 1, 1, 1, 1, 1, 1, 4 ),
 ( 0.000000000000000000, 0.07315862907712983310, 0.1430989967074559055, 0.2105333571262071879, 0.2759142635903734653, 0.3397077151413689933, 0.4013946392018796772, 0.4627937533375801049, 0.5237250720276656057, 0.5836284080752294212, 0.6425725562371763511, 0.7010486867616194662, 0.7591976973140022178, 0.8177727706511607186, 0.8769111530050104353, 0.9375229829315941954, 1.000000000000000000 ),
 .UNSPECIFIED. ) ;
#5090 = CARTESIAN_POINT ( 'NONE',  ( 2.500000000000000000, -1.574999999999999734, -3.061616997868383141E-16 ) ) ;
#5091 = DIRECTION ( 'NONE',  ( 0.9569724629708533659, 0.000000000000000000, -0.2901787468363226097 ) ) ;
#5092 = DIRECTION ( 'NONE',  ( -0.000000000000000000, 1.000000000000000000, -0.000000000000000000 ) ) ;
#5093 = VECTOR ( 'NONE', #6756, 1000.000000000000000 ) ;
#5094 = CARTESIAN_POINT ( 'NONE',  ( 0.000000000000000000, 100.0000000000000000, 0.000000000000000000 ) ) ;
#5095 = ORIENTED_EDGE ( 'NONE', *, *, #6474, .T. ) ;
#5096 = LINE ( 'NONE', #1074, #5223 ) ;
#5097 = CARTESIAN_POINT ( 'NONE',  ( -11.36312591709335962, 3.799999998907525711, -27.43301270000000258 ) ) ;
#5098 = CARTESIAN_POINT ( 'NONE',  ( 3.061616997868383043E-15, 97.50000000000000000, 25.00000000000000000 ) ) ;
#5099 = CARTESIAN_POINT ( 'NONE',  ( -1.249999999999998224, -4.424999999999998934, 2.165063509461097713 ) ) ;
#5100 = CARTESIAN_POINT ( 'NONE',  ( 7.753999887479250397, 99.50000000000000000, 20.97676509141502166 ) ) ;
#5101 = CARTESIAN_POINT ( 'NONE',  ( 3.207057600658871355, 99.50000000000000000, -22.07913334414698880 ) ) ;
#5102 = CARTESIAN_POINT ( 'NONE',  ( 11.18376618407356915, 5.549999997815052488, -27.00000000000000355 ) ) ;
#5103 = EDGE_CURVE ( 'NONE', #7275, #4897, #7677, .T. ) ;
#5104 = CARTESIAN_POINT ( 'NONE',  ( 3.061616997868383141E-16, -15.00000000000000000, 2.500000000000000000 ) ) ;
#5105 = CARTESIAN_POINT ( 'NONE',  ( 1.249999999999999334, -4.593749998770965348, -2.165063509461096825 ) ) ;
#5106 = CARTESIAN_POINT ( 'NONE',  ( -1.249999999999998224, -0.3749999999999999445, 2.165063509461097713 ) ) ;
#5107 = EDGE_CURVE ( 'NONE', #7571, #3495, #469, .T. ) ;
#5108 = CARTESIAN_POINT ( 'NONE',  ( -22.05902956123343017, 99.50000000000000000, -10.96257574645357558 ) ) ;
#5109 = DIRECTION ( 'NONE',  ( 0.000000000000000000, 0.000000000000000000, -1.000000000000000000 ) ) ;
#5110 = DIRECTION ( 'NONE',  ( 0.000000000000000000, 0.000000000000000000, 1.000000000000000000 ) ) ;
#5111 = AXIS2_PLACEMENT_3D ( 'NONE', #9852, #971, #7346 ) ;
#5112 = CIRCLE ( 'NONE', #7005, 2.062556682370379590 ) ;
#5113 = CARTESIAN_POINT ( 'NONE',  ( 1.249999999999999334, -0.5999999999999999778, -2.165063509461096825 ) ) ;
#5114 = SHAPE_REPRESENTATION ( 'o-rings series a_iso_O-ring 45x2.65-A-ISO 3601-1', ( #5055 ), #3636 ) ;
#5115 = DIRECTION ( 'NONE',  ( 0.000000000000000000, 0.000000000000000000, 1.000000000000000000 ) ) ;
#5116 = DIRECTION ( 'NONE',  ( 0.9567904646982170469, 0.000000000000000000, -0.2907782774943306059 ) ) ;
#5117 = LINE ( 'NONE', #3396, #3889 ) ;
#5118 = CARTESIAN_POINT ( 'NONE',  ( -27.43301270000000258, 3.049999998907525267, -3.359575119402369376E-15 ) ) ;
#5119 = CARTESIAN_POINT ( 'NONE',  ( -19.39806930854667755, 0.6499999989075252449, -19.39806930854668110 ) ) ;
#5120 = AXIS2_PLACEMENT_3D ( 'NONE', #3506, #6692, #7528 ) ;
#5121 = DIRECTION ( 'NONE',  ( -0.000000000000000000, 1.000000000000000000, -0.000000000000000000 ) ) ;
#5122 = APPLICATION_CONTEXT ( 'automotive_design' ) ;
#5123 = CARTESIAN_POINT ( 'NONE',  ( 4.693123912524271191, 100.0000000000000284, -24.12247278045041554 ) ) ;
#5124 = CARTESIAN_POINT ( 'NONE',  ( 7.978247738654171251, 100.0000000000000000, 20.00924965157036794 ) ) ;
#5125 = CARTESIAN_POINT ( 'NONE',  ( 8.429066232339796017, 99.50000000000000000, 19.67794530653910101 ) ) ;
#5126 = CARTESIAN_POINT ( 'NONE',  ( -9.703070624755296135E-15, -3.937500000000000888, 2.500000000000000444 ) ) ;
#5127 = LINE ( 'NONE', #6551, #7444 ) ;
#5128 = CARTESIAN_POINT ( 'NONE',  ( -15.69732130854469432, 99.50000000000001421, 15.19348709373450035 ) ) ;
#5129 = FILL_AREA_STYLE ('',( #1056 ) ) ;
#5130 = CARTESIAN_POINT ( 'NONE',  ( 11.18376618407357626, 4.650000000000000355, 27.00000000000000000 ) ) ;
#5131 = PRODUCT_DEFINITION_FORMATION_WITH_SPECIFIED_SOURCE ( 'ANY', '', #5693, .NOT_KNOWN. ) ;
#5132 = CARTESIAN_POINT ( 'NONE',  ( 9.526713201929464248, 99.99999999999994316, 20.38668308130821671 ) ) ;
#5133 = LINE ( 'NONE', #7591, #2771 ) ;
#5134 = ORIENTED_EDGE ( 'NONE', *, *, #3091, .F. ) ;
#5135 = CARTESIAN_POINT ( 'NONE',  ( -16.30427144417478402, 99.49999999999998579, 16.48895498912494517 ) ) ;
#5136 = CARTESIAN_POINT ( 'NONE',  ( 2.256430356249999658, -1.340624999385482852, -1.302750673588581432 ) ) ;
#5137 = VERTEX_POINT ( 'NONE', #577 ) ;
#5138 = CARTESIAN_POINT ( 'NONE',  ( -22.33589105551819642, 99.50000000000002842, -11.18147695539509812 ) ) ;
#5139 = LINE ( 'NONE', #4359, #2965 ) ;
#5140 = CARTESIAN_POINT ( 'NONE',  ( -11.18376618407358336, 5.149999997815050357, 26.99999999999999645 ) ) ;
#5141 = CARTESIAN_POINT ( 'NONE',  ( -15.10687288066601930, 99.99999999999998579, 15.84109048427130517 ) ) ;
#5142 = EDGE_CURVE ( 'NONE', #2986, #1777, #3426, .T. ) ;
#5143 = ADVANCED_FACE ( 'NONE', ( #104 ), #8793, .T. ) ;
#5144 = ORIENTED_EDGE ( 'NONE', *, *, #9143, .F. ) ;
#5145 = FACE_OUTER_BOUND ( 'NONE', #2687, .T. ) ;
#5146 = CARTESIAN_POINT ( 'NONE',  ( -2.500000000000000000, -0.8437499987709659033, 0.000000000000000000 ) ) ;
#5147 = CARTESIAN_POINT ( 'NONE',  ( -22.05902956123343017, 100.0000000000000000, -10.96257574645357558 ) ) ;
#5148 = DIRECTION ( 'NONE',  ( -0.000000000000000000, 1.000000000000000000, -0.000000000000000000 ) ) ;
#5149 = ORIENTED_EDGE ( 'NONE', *, *, #7717, .T. ) ;
#5150 = FACE_OUTER_BOUND ( 'NONE', #3749, .T. ) ;
#5151 = CARTESIAN_POINT ( 'NONE',  ( 19.39806930854668110, 5.249999998907525445, -19.39806930854668110 ) ) ;
#5152 = CARTESIAN_POINT ( 'NONE',  ( -2.500000000000000000, -4.949999999999999289, 0.000000000000000000 ) ) ;
#5153 = CARTESIAN_POINT ( 'NONE',  ( 3.824506687597884369, 99.50000000000002842, -24.68145443631992109 ) ) ;
#5154 = CARTESIAN_POINT ( 'NONE',  ( 7.771508748547515388, 99.99999999999995737, 20.40818475981234315 ) ) ;
#5155 = ORIENTED_EDGE ( 'NONE', *, *, #5638, .F. ) ;
#5156 = CARTESIAN_POINT ( 'NONE',  ( 9.692323321704657602, 99.50000000000001421, 21.58969587442354410 ) ) ;
#5157 = CARTESIAN_POINT ( 'NONE',  ( -27.00000000000000355, 2.549999997815051156, -11.18376618407357093 ) ) ;
#5158 = LINE ( 'NONE', #3089, #4520 ) ;
#5159 = CARTESIAN_POINT ( 'NONE',  ( -21.18972881998075763, 99.99999999999998579, -9.781869222470191971 ) ) ;
#5160 = CARTESIAN_POINT ( 'NONE',  ( 0.000000000000000000, 100.0000000000000000, 0.000000000000000000 ) ) ;
#5161 = ORIENTED_EDGE ( 'NONE', *, *, #1641, .F. ) ;
#5162 = CARTESIAN_POINT ( 'NONE',  ( 2.843562173796539749, 100.0000000000000142, -21.91597968833000110 ) ) ;
#5163 = CARTESIAN_POINT ( 'NONE',  ( -0.6698729810778069060, -2.342403810567665445, -2.500000000000000000 ) ) ;
#5164 = ORIENTED_EDGE ( 'NONE', *, *, #9274, .F. ) ;
#5165 = CARTESIAN_POINT ( 'NONE',  ( -2.499999999999999556, -1.312500000000000000, 1.443375672974065882 ) ) ;
#5166 = EDGE_CURVE ( 'NONE', #2280, #8581, #6763, .T. ) ;
#5167 = APPLICATION_PROTOCOL_DEFINITION ( 'draft international standard', 'automotive_design', 1998, #451 ) ;
#5168 = CARTESIAN_POINT ( 'NONE',  ( -14.83363727892122519, 99.50000000000001421, 15.50654517199034466 ) ) ;
#5169 = CARTESIAN_POINT ( 'NONE',  ( 2.940192896829773250, 100.0000000000000142, -23.44521981770616037 ) ) ;
#5170 = CARTESIAN_POINT ( 'NONE',  ( -27.43301270000000258, 3.849999998907525534, -3.359575119402369376E-15 ) ) ;
#5171 = CARTESIAN_POINT ( 'NONE',  ( -4.959819536546781389E-15, 0.6000000000000000888, 27.00000000000000355 ) ) ;
#5172 = CARTESIAN_POINT ( 'NONE',  ( -16.25490828497592588, 99.99999999999998579, 14.91257814242970348 ) ) ;
#5173 = DIRECTION ( 'NONE',  ( 0.000000000000000000, 0.000000000000000000, 1.000000000000000000 ) ) ;
#5174 = SURFACE_STYLE_FILL_AREA ( #5862 ) ;
#5175 =( BOUNDED_CURVE ( )  B_SPLINE_CURVE ( 2, ( #6822, #6264, #6991, #3696, #8568, #10196, #1338, #7720, #9463 ),
 .UNSPECIFIED., .F., .F. ) 
 B_SPLINE_CURVE_WITH_KNOTS ( ( 3, 2, 2, 2, 3 ),
 ( 0.1071428571428571369, 0.1250000000000000000, 0.1428571428571428492, 0.1607142857142857262, 0.1785714285714285754 ),
 .UNSPECIFIED. ) 
 CURVE ( )  GEOMETRIC_REPRESENTATION_ITEM ( )  RATIONAL_B_SPLINE_CURVE ( ( 1.000000000000000000, 0.9238795325112867385, 1.000000000000000000, 0.9238795325112867385, 1.000000000000000000, 0.9238795325112867385, 1.000000000000000000, 0.9238795325112867385, 1.000000000000000000 ) ) 
 REPRESENTATION_ITEM ( '' )  );
#5176 = CARTESIAN_POINT ( 'NONE',  ( -21.39817337045129619, 99.50000000000001421, -9.317726141196148504 ) ) ;
#5177 = CARTESIAN_POINT ( 'NONE',  ( -21.56977948371741505, 99.49999999999995737, -11.44450812306045329 ) ) ;
#5178 = EDGE_LOOP ( 'NONE', ( #9549, #2245, #8310, #6459 ) ) ;
#5179 = FACE_BOUND ( 'NONE', #3402, .T. ) ;
#5180 = FACE_OUTER_BOUND ( 'NONE', #5911, .T. ) ;
#5181 = SURFACE_STYLE_FILL_AREA ( #8132 ) ;
#5182 = CARTESIAN_POINT ( 'NONE',  ( -0.6698729810778054627, -1.651346188203300036, 2.500000000000000000 ) ) ;
#5183 = B_SPLINE_CURVE_WITH_KNOTS ( 'NONE', 3,
 ( #4842, #3409, #4894, #1598, #2585, #3364, #4938, #9795, #6512, #5583, #9654, #8771, #176, #8089, #1741, #919, #8822, #8037, #9701 ),
 .UNSPECIFIED., .F., .F.,
 ( 4, 1, 1, 1, 1, 1, 1, 1, 1, 1, 1, 1, 1, 1, 1, 1, 4 ),
 ( 0.000000000000000000, 0.06282509715607415002, 0.1231380613775250599, 0.1822388757841713336, 0.2396184841454026548, 0.2973605923678978580, 0.3541959668311244203, 0.4122907788200148582, 0.4717534157231769720, 0.5322282553174864095, 0.5926403291039165078, 0.6546871955647078911, 0.7179012776534754448, 0.7839155840457150415, 0.8527518695723632636, 0.9242989153657757972, 1.000000000000000000 ),
 .UNSPECIFIED. ) ;
#5184 = ADVANCED_FACE ( 'NONE', ( #4813 ), #6281, .T. ) ;
#5185 = CARTESIAN_POINT ( 'NONE',  ( 9.563602730896748838, 99.99999999999994316, 20.87184380654744587 ) ) ;
#5186 = AXIS2_PLACEMENT_3D ( 'NONE', #830, #1507, #2243 ) ;
#5187 = CARTESIAN_POINT ( 'NONE',  ( -21.31369174262763622, 99.99999999999997158, -9.710155485040722567 ) ) ;
#5188 = ORIENTED_EDGE ( 'NONE', *, *, #6474, .F. ) ;
#5189 = CARTESIAN_POINT ( 'NONE',  ( -21.16695614262292580, 99.50000000000000000, -11.33496398805607441 ) ) ;
#5190 = CARTESIAN_POINT ( 'NONE',  ( 2.256430356250000102, -2.728124999385482585, -2.763330213280484622E-16 ) ) ;
#5191 = EDGE_LOOP ( 'NONE', ( #2888, #6195, #508, #2265 ) ) ;
#5192 = DIRECTION ( 'NONE',  ( 0.000000000000000000, -1.000000000000000000, 0.000000000000000000 ) ) ;
#5193 = CARTESIAN_POINT ( 'NONE',  ( 19.39806930854667399, 0.9499999989075252893, 19.39806930854668465 ) ) ;
#5194 = CARTESIAN_POINT ( 'NONE',  ( 2.781278341185189795, -20.00000000000000000, 1.353213781785882031 ) ) ;
#5195 = CARTESIAN_POINT ( 'NONE',  ( -15.11611088805441661, 100.0000000000000000, 16.06180012866831319 ) ) ;
#5196 = ORIENTED_EDGE ( 'NONE', *, *, #4019, .F. ) ;
#5197 = CARTESIAN_POINT ( 'NONE',  ( -1.767625397874844694E-16, -0.5062499987709657701, -2.886751345948128655 ) ) ;
#5198 = CARTESIAN_POINT ( 'NONE',  ( -16.79604063091391097, 100.0000000000000000, 15.40463673182947701 ) ) ;
#5199 = CARTESIAN_POINT ( 'NONE',  ( -15.07178375341841381, 100.0000000000000000, 16.66969090848992607 ) ) ;
#5200 = EDGE_LOOP ( 'NONE', ( #1536, #9622, #9646, #7764, #808, #3401, #7707 ) ) ;
#5201 = CARTESIAN_POINT ( 'NONE',  ( 5.243816414761435674, 99.50000000000000000, -23.48558366465980995 ) ) ;
#5202 = CARTESIAN_POINT ( 'NONE',  ( -1.915120254295647362, -5.000523192925935945, -1.606958123781256464 ) ) ;
#5203 = AXIS2_PLACEMENT_3D ( 'NONE', #4286, #6741, #7470 ) ;
#5204 = CARTESIAN_POINT ( 'NONE',  ( -16.65546786808457469, 99.99999999999998579, 16.57295196178722918 ) ) ;
#5205 = ORIENTED_EDGE ( 'NONE', *, *, #9048, .T. ) ;
#5206 = CARTESIAN_POINT ( 'NONE',  ( 1.679787559701184688E-15, 5.349999998907525089, -27.43301270000000258 ) ) ;
#5207 = FACE_OUTER_BOUND ( 'NONE', #1613, .T. ) ;
#5208 = DIRECTION ( 'NONE',  ( 0.000000000000000000, -1.000000000000000000, 0.000000000000000000 ) ) ;
#5209 = CARTESIAN_POINT ( 'NONE',  ( -16.63177974700816009, 99.50000000000000000, 16.59747536361813403 ) ) ;
#5210 = CARTESIAN_POINT ( 'NONE',  ( -3.061616997868383634E-16, -20.00000000000000000, 2.500000000000000444 ) ) ;
#5211 = VECTOR ( 'NONE', #6669, 1000.000000000000114 ) ;
#5212 = EDGE_LOOP ( 'NONE', ( #5, #3243, #2058, #1207 ) ) ;
#5213 = CARTESIAN_POINT ( 'NONE',  ( -16.05932294508833280, 100.0000000000000000, 15.21084698918278555 ) ) ;
#5214 = CARTESIAN_POINT ( 'NONE',  ( 19.39806930854667399, 2.649999998907525356, 19.39806930854668465 ) ) ;
#5215 = ORIENTED_EDGE ( 'NONE', *, *, #3681, .T. ) ;
#5216 = ADVANCED_FACE ( 'NONE', ( #1619 ), #2260, .T. ) ;
#5217 = CARTESIAN_POINT ( 'NONE',  ( -1.767625397874844694E-16, -2.362499999999999822, -2.886751345948128655 ) ) ;
#5218 = CARTESIAN_POINT ( 'NONE',  ( 1.250000000000001110, -3.899999999999999911, 2.165063509461096380 ) ) ;
#5219 = CARTESIAN_POINT ( 'NONE',  ( -1.128215178125000273, -2.578124999385482674, -1.954126010382871259 ) ) ;
#5220 = COLOUR_RGB ( '',1.000000000000000000, 0.9490196078431372140, 0.9098039215686274384 ) ;
#5221 = CARTESIAN_POINT ( 'NONE',  ( -11.36312591709335962, 2.899999998907525356, -27.43301270000000258 ) ) ;
#5222 = CARTESIAN_POINT ( 'NONE',  ( 0.6698729810778075722, -0.7111538093386315929, 2.499999999999999556 ) ) ;
#5223 = VECTOR ( 'NONE', #8296, 1000.000000000000000 ) ;
#5224 = ORIENTED_EDGE ( 'NONE', *, *, #5883, .F. ) ;
#5225 = CARTESIAN_POINT ( 'NONE',  ( 4.996790860652426159E-15, -1.912499999999999867, -2.500000000000000000 ) ) ;
#5226 = PLANE ( 'NONE',  #2637 ) ;
#5227 = CARTESIAN_POINT ( 'NONE',  ( 8.393217272293057363, 100.0000000000000000, 19.69436072183531650 ) ) ;
#5228 = CARTESIAN_POINT ( 'NONE',  ( -15.56095293356939813, 100.0000000000000142, 15.23332223661997453 ) ) ;
#5229 = CARTESIAN_POINT ( 'NONE',  ( -2.256430356249998770, -1.453124999385482896, 1.302750673588581876 ) ) ;
#5230 = CARTESIAN_POINT ( 'NONE',  ( -1.915118561403101660, -5.394273269507307234, -1.606960141313192203 ) ) ;
#5231 = EDGE_LOOP ( 'NONE', ( #5196, #5149, #3519, #503 ) ) ;
#5232 = CARTESIAN_POINT ( 'NONE',  ( 1.128215178125001161, -0.8906249993854827851, 1.954126010382870815 ) ) ;
#5233 = CARTESIAN_POINT ( 'NONE',  ( -11.36312591709337383, 0.7999999989075252671, 27.43301269999999548 ) ) ;
#5234 = CARTESIAN_POINT ( 'NONE',  ( -16.25490828497592588, 99.99999999999994316, 14.91257814242970348 ) ) ;
#5235 = CARTESIAN_POINT ( 'NONE',  ( -22.57971655928959365, 100.0000000000000000, -10.84768434062017839 ) ) ;
#5236 = B_SPLINE_CURVE_WITH_KNOTS ( 'NONE', 3,
 ( #9279, #656, #549, #3686, #5427, #2903, #6870, #1440, #1330, #5306, #3635 ),
 .UNSPECIFIED., .F., .F.,
 ( 4, 1, 1, 1, 1, 1, 1, 1, 4 ),
 ( 0.000000000000000000, 0.09809051273808343241, 0.1997563395654988194, 0.3058527769869914259, 0.4162847437678430240, 0.5377099880548563693, 0.6743560419832976827, 0.8289895874771281425, 1.000000000000000000 ),
 .UNSPECIFIED. ) ;
#5237 = CARTESIAN_POINT ( 'NONE',  ( 0.000000000000000000, 5.000000000000000000, 0.000000000000000000 ) ) ;
#5238 = ORIENTED_EDGE ( 'NONE', *, *, #4397, .T. ) ;
#5239 =( BOUNDED_SURFACE ( )  B_SPLINE_SURFACE ( 1, 2, ( 
 ( #4238, #312, #2717, #9101, #7419, #9155, #8368, #4390, #7575, #413, #3609, #9732, #5764, #4188, #3045, #9250, #525, #10039, #2198, #8476, #9426, #5452, #7850, #6225, #6955, #4494, #2253, #6844, #10158, #8643, #8531, #7007, #1467, #10211, #1250, #7686, #3664, #3715, #8590, #5341, #680, #2083, #4660, #5398, #6792, #9991, #10094, #468, #5277, #1356, #7796, #2875, #6059, #9369, #4440, #2025, #2827, #4548, #6007, #7742, #1304, #9200, #5219, #576, #6898, #2991, #8419, #2140, #7628, #2933, #6115, #1411, #9308, #3769, #6171, #4604, #627, #3826, #4810, #8054, #5703, #8743, #1567, #46, #6336, #4030, #2354, #6484, #7115, #3199, #3293, #8007, #9479, #6433, #6381, #4812, #9674, #10315, #838, #7059, #2458, #4757, #3152, #1618, #7212, #5506, #2512, #9530, #7955, #5551, #3246, #788, #2306, #8695, #9626, #2406, #3980, #5654, #1516, #9574, #8844, #3099, #4709, #7902, #735, #1670, #7165, #3873, #4864, #5602, #889, #8792, #3928, #4079, #7261 ),
 ( #6283, #102, #8890, #1715, #4911, #8108, #10267, #8572, #719, #8680, #9353, #8629, #7669, #5381, #3752, #2124, #6268, #6882, #3700, #9465, #666, #10079, #3860, #10253, #611, #7046, #5323, #10199, #2976, #506, #7837, #2341, #6323, #1452, #3914, #2915, #6098, #4645, #7780, #7099, #1342, #1398, #3811, #6995, #9516, #3084, #2293, #9291, #3034, #5490, #8513, #1503, #4529, #4587, #4699, #1287, #7887, #10304, #6210, #7725, #560, #6938, #10139, #3136, #9408, #4477, #8458, #6156, #2182, #2237, #5439, #975, #3284, #3186, #4944, #7994, #7304, #8043, #4120, #9565, #7251, #30, #7942, #4902, #9756, #3371, #5692, #4165, #775, #4745, #1703, #4850, #7349, #8778, #5640, #876, #4067, #6565, #141, #3331, #3966, #89, #8097, #2396, #926, #5592, #8831, #5739, #8732, #8881, #9709, #1659, #4795, #1605, #826, #4018, #186, #6473, #1555, #2547, #6519, #8928, #5541, #9663, #7152, #2498, #6371, #8146, #7202, #3234, #1748, #10355, #6422, #9612, #2445 ) ),
 .UNSPECIFIED., .F., .F., .F. ) 
 B_SPLINE_SURFACE_WITH_KNOTS ( ( 2, 2 ),
 ( 3, 2, 2, 2, 2, 2, 2, 2, 2, 2, 2, 2, 2, 2, 2, 2, 2, 2, 2, 2, 2, 2, 2, 2, 2, 2, 2, 2, 2, 2, 2, 2, 2, 2, 2, 2, 2, 2, 2, 2, 2, 2, 2, 2, 2, 2, 2, 2, 2, 2, 2, 2, 2, 2, 2, 2, 2, 2, 2, 2, 2, 2, 2, 2, 2, 2, 2, 3 ),
 ( 0.000000000000000000, 1.000000000000000000 ),
 ( 0.000000000000000000, 0.01388888888888888812, 0.02777777777777777624, 0.04166666666666666435, 0.05555555555555555247, 0.06944444444444444753, 0.08333333333333332871, 0.09722222222222222376, 0.1111111111111111049, 0.1250000000000000000, 0.1388888888888888951, 0.1527777777777777901, 0.1666666666666666574, 0.1805555555555555525, 0.1944444444444444475, 0.2083333333333333426, 0.2222222222222222099, 0.2361111111111111049, 0.2500000000000000000, 0.2638888888888888951, 0.2777777777777777901, 0.2916666666666666852, 0.3055555555555555802, 0.3194444444444444198, 0.3333333333333333148, 0.3472222222222222099, 0.3611111111111111049, 0.3750000000000000000, 0.3888888888888888951, 0.4027777777777777901, 0.4166666666666666852, 0.4305555555555555802, 0.4444444444444444198, 0.4583333333333333148, 0.4722222222222222099, 0.4861111111111111049, 0.5000000000000000000, 0.5138888888888888395, 0.5277777777777777901, 0.5416666666666666297, 0.5555555555555555802, 0.5694444444444444198, 0.5833333333333333703, 0.5972222222222222099, 0.6111111111111111605, 0.6250000000000000000, 0.6388888888888888395, 0.6527777777777777901, 0.6666666666666666297, 0.6805555555555555802, 0.6944444444444444198, 0.7083333333333333703, 0.7222222222222222099, 0.7361111111111111605, 0.7500000000000000000, 0.7638888888888888395, 0.7777777777777777901, 0.7916666666666666297, 0.8055555555555555802, 0.8194444444444444198, 0.8333333333333333703, 0.8472222222222222099, 0.8611111111111111605, 0.8750000000000000000, 0.8888888888888888395, 0.9027777777777777901, 0.9166666666666666297, 0.9258785565094815873 ),
 .UNSPECIFIED. ) 
 GEOMETRIC_REPRESENTATION_ITEM ( )  RATIONAL_B_SPLINE_SURFACE ( (
 ( 1.000000000000000000, 0.8660254037844387076, 1.000000000000000000, 0.8660254037844387076, 1.000000000000000000, 0.8660254037844387076, 1.000000000000000000, 0.8660254037844387076, 1.000000000000000000, 0.8660254037844387076, 1.000000000000000000, 0.8660254037844387076, 1.000000000000000000, 0.8660254037844387076, 1.000000000000000000, 0.8660254037844387076, 1.000000000000000000, 0.8660254037844387076, 1.000000000000000000, 0.8660254037844387076, 1.000000000000000000, 0.8660254037844387076, 1.000000000000000000, 0.8660254037844387076, 1.000000000000000000, 0.8660254037844387076, 1.000000000000000000, 0.8660254037844387076, 1.000000000000000000, 0.8660254037844387076, 1.000000000000000000, 0.8660254037844387076, 1.000000000000000000, 0.8660254037844387076, 1.000000000000000000, 0.8660254037844387076, 1.000000000000000000, 0.8660254037844387076, 1.000000000000000000, 0.8660254037844387076, 1.000000000000000000, 0.8660254037844387076, 1.000000000000000000, 0.8660254037844387076, 1.000000000000000000, 0.8660254037844387076, 1.000000000000000000, 0.8660254037844387076, 1.000000000000000000, 0.8660254037844387076, 1.000000000000000000, 0.8660254037844387076, 1.000000000000000000, 0.8660254037844387076, 1.000000000000000000, 0.8660254037844387076, 1.000000000000000000, 0.8660254037844387076, 1.000000000000000000, 0.8660254037844387076, 1.000000000000000000, 0.8660254037844387076, 1.000000000000000000, 0.8660254037844387076, 1.000000000000000000, 0.8660254037844387076, 1.000000000000000000, 0.8660254037844387076, 1.000000000000000000, 0.8660254037844387076, 1.000000000000000000, 0.8660254037844387076, 1.000000000000000000, 0.8660254037844387076, 1.000000000000000000, 0.8660254037844387076, 1.000000000000000000, 0.8660254037844387076, 1.000000000000000000, 0.8660254037844387076, 1.000000000000000000, 0.8660254037844387076, 1.000000000000000000, 0.8660254037844387076, 1.000000000000000000, 0.8660254037844387076, 1.000000000000000000, 0.8660254037844387076, 1.000000000000000000, 0.8660254037844387076, 1.000000000000000000, 0.8660254037844387076, 1.000000000000000000, 0.8660254037844387076, 1.000000000000000000, 0.8660254037844387076, 1.000000000000000000, 0.8660254037844387076, 1.000000000000000000, 0.8660254037844387076, 1.000000000000000000, 0.8660254037844387076, 1.000000000000000000, 0.8660254037844387076, 1.000000000000000000, 0.8660254037844387076, 1.000000000000000000, 0.8660254037844387076, 1.000000000000000000, 0.8660254037844387076, 1.000000000000000000, 0.8660254037844387076, 1.000000000000000000, 0.8660254037844387076, 1.000000000000000000, 0.8660254037844387076, 1.000000000000000000, 0.8660254037844387076, 1.000000000000000000, 0.8660254037844387076, 1.000000000000000000, 0.8660254037844387076, 1.000000000000000000, 0.8660254037844387076, 1.000000000000000000, 0.8660254037844387076, 1.000000000000000000, 0.8660254037844387076, 1.000000000000000000, 0.8660254037844387076, 1.000000000000000000, 0.8660254037844387076, 1.000000000000000000, 0.9111405360107182050, 0.9401542295229976531),
 ( 1.000000000000000000, 0.8660254037844387076, 1.000000000000000000, 0.8660254037844387076, 1.000000000000000000, 0.8660254037844387076, 1.000000000000000000, 0.8660254037844387076, 1.000000000000000000, 0.8660254037844387076, 1.000000000000000000, 0.8660254037844387076, 1.000000000000000000, 0.8660254037844387076, 1.000000000000000000, 0.8660254037844387076, 1.000000000000000000, 0.8660254037844387076, 1.000000000000000000, 0.8660254037844387076, 1.000000000000000000, 0.8660254037844387076, 1.000000000000000000, 0.8660254037844387076, 1.000000000000000000, 0.8660254037844387076, 1.000000000000000000, 0.8660254037844387076, 1.000000000000000000, 0.8660254037844387076, 1.000000000000000000, 0.8660254037844387076, 1.000000000000000000, 0.8660254037844387076, 1.000000000000000000, 0.8660254037844387076, 1.000000000000000000, 0.8660254037844387076, 1.000000000000000000, 0.8660254037844387076, 1.000000000000000000, 0.8660254037844387076, 1.000000000000000000, 0.8660254037844387076, 1.000000000000000000, 0.8660254037844387076, 1.000000000000000000, 0.8660254037844387076, 1.000000000000000000, 0.8660254037844387076, 1.000000000000000000, 0.8660254037844387076, 1.000000000000000000, 0.8660254037844387076, 1.000000000000000000, 0.8660254037844387076, 1.000000000000000000, 0.8660254037844387076, 1.000000000000000000, 0.8660254037844387076, 1.000000000000000000, 0.8660254037844387076, 1.000000000000000000, 0.8660254037844387076, 1.000000000000000000, 0.8660254037844387076, 1.000000000000000000, 0.8660254037844387076, 1.000000000000000000, 0.8660254037844387076, 1.000000000000000000, 0.8660254037844387076, 1.000000000000000000, 0.8660254037844387076, 1.000000000000000000, 0.8660254037844387076, 1.000000000000000000, 0.8660254037844387076, 1.000000000000000000, 0.8660254037844387076, 1.000000000000000000, 0.8660254037844387076, 1.000000000000000000, 0.8660254037844387076, 1.000000000000000000, 0.8660254037844387076, 1.000000000000000000, 0.8660254037844387076, 1.000000000000000000, 0.8660254037844387076, 1.000000000000000000, 0.8660254037844387076, 1.000000000000000000, 0.8660254037844387076, 1.000000000000000000, 0.8660254037844387076, 1.000000000000000000, 0.8660254037844387076, 1.000000000000000000, 0.8660254037844387076, 1.000000000000000000, 0.8660254037844387076, 1.000000000000000000, 0.8660254037844387076, 1.000000000000000000, 0.8660254037844387076, 1.000000000000000000, 0.8660254037844387076, 1.000000000000000000, 0.8660254037844387076, 1.000000000000000000, 0.8660254037844387076, 1.000000000000000000, 0.8660254037844387076, 1.000000000000000000, 0.8660254037844387076, 1.000000000000000000, 0.8660254037844387076, 1.000000000000000000, 0.8660254037844387076, 1.000000000000000000, 0.8660254037844387076, 1.000000000000000000, 0.8660254037844387076, 1.000000000000000000, 0.8660254037844387076, 1.000000000000000000, 0.8660254037844387076, 1.000000000000000000, 0.8660254037844387076, 1.000000000000000000, 0.8660254037844387076, 1.000000000000000000, 0.9111405360107182050, 0.9401542295229976531) ) ) 
 REPRESENTATION_ITEM ( '' )  SURFACE ( )  );
#5240 = FACE_OUTER_BOUND ( 'NONE', #6, .T. ) ;
#5241 = ADVANCED_FACE ( 'NONE', ( #3294 ), #2342, .T. ) ;
#5242 = CARTESIAN_POINT ( 'NONE',  ( -1.595409442497313560E-16, -0.8156249993854829405, -2.605501347177161087 ) ) ;
#5243 = VERTEX_POINT ( 'NONE', #9038 ) ;
#5244 = EDGE_CURVE ( 'NONE', #7666, #5650, #9052, .T. ) ;
#5245 = CARTESIAN_POINT ( 'NONE',  ( -22.33529725360453000, 99.99999999999994316, -10.20112572733487255 ) ) ;
#5246 = FACE_OUTER_BOUND ( 'NONE', #1324, .T. ) ;
#5247 = AXIS2_PLACEMENT_3D ( 'NONE', #9442, #7761, #6972 ) ;
#5248 = DIRECTION ( 'NONE',  ( -0.000000000000000000, -1.000000000000000000, -0.000000000000000000 ) ) ;
#5249 = DIRECTION ( 'NONE',  ( 0.05376826219280737146, 0.000000000000000000, 0.9985534407235125975 ) ) ;
#5250 = CARTESIAN_POINT ( 'NONE',  ( 4.850954546176396320, 99.49999999999998579, -24.43907202982397209 ) ) ;
#5251 = EDGE_LOOP ( 'NONE', ( #3019, #9847, #8245, #8860, #5079 ) ) ;
#5252 = CARTESIAN_POINT ( 'NONE',  ( 2.939152317953647500E-15, 75.00000000000001421, -23.99999999999999645 ) ) ;
#5253 = AXIS2_PLACEMENT_3D ( 'NONE', #2127, #1400, #2069 ) ;
#5254 = CARTESIAN_POINT ( 'NONE',  ( -16.62994343074595349, 99.99999999999998579, 15.18287566599475191 ) ) ;
#5255 = DIRECTION ( 'NONE',  ( 0.000000000000000000, 0.000000000000000000, -1.000000000000000000 ) ) ;
#5256 = ORIENTED_EDGE ( 'NONE', *, *, #4784, .T. ) ;
#5257 = CARTESIAN_POINT ( 'NONE',  ( 27.00000000000000355, 1.449999997815050401, -11.18376618407356915 ) ) ;
#5258 = CARTESIAN_POINT ( 'NONE',  ( 27.43301270000000258, 2.799999998907525267, -11.36312591709336139 ) ) ;
#5259 = CARTESIAN_POINT ( 'NONE',  ( -1.249999999999998224, -4.875000000000000000, 2.165063509461097713 ) ) ;
#5260 =( REPRESENTATION_RELATIONSHIP ('NONE','NONE', #3375, #1584 ) REPRESENTATION_RELATIONSHIP_WITH_TRANSFORMATION ( #836 )SHAPE_REPRESENTATION_RELATIONSHIP( ) );
#5261 = CARTESIAN_POINT ( 'NONE',  ( 21.79306891025641235, 99.50000000000000000, -1.065004006410256387 ) ) ;
#5262 = VECTOR ( 'NONE', #998, 1000.000000000000000 ) ;
#5263 = ORIENTED_EDGE ( 'NONE', *, *, #6476, .T. ) ;
#5264 = CARTESIAN_POINT ( 'NONE',  ( 9.820792995160308791, 99.50000000000000000, 20.21220011423140761 ) ) ;
#5265 = CARTESIAN_POINT ( 'NONE',  ( 4.503533123526070270, 99.49999999999995737, -24.63026223303895890 ) ) ;
#5266 = CARTESIAN_POINT ( 'NONE',  ( -9.703070624755296135E-15, -3.881249998770965881, 2.500000000000000444 ) ) ;
#5267 = CARTESIAN_POINT ( 'NONE',  ( -16.52157078939288937, 99.49999999999998579, 16.20087177393598665 ) ) ;
#5268 = LINE ( 'NONE', #3125, #7074 ) ;
#5269 = ORIENTED_EDGE ( 'NONE', *, *, #9785, .T. ) ;
#5270 = CARTESIAN_POINT ( 'NONE',  ( -16.56928979259283352, 100.0000000000000284, 16.65656195153832897 ) ) ;
#5271 = CARTESIAN_POINT ( 'NONE',  ( 1.679787559701184688E-15, 0.5499999989075251561, -27.43301270000000258 ) ) ;
#5272 = VERTEX_POINT ( 'NONE', #6779 ) ;
#5273 = CARTESIAN_POINT ( 'NONE',  ( 2.500000000000000000, -2.474999999999999645, -3.061616997868383141E-16 ) ) ;
#5274 = DIRECTION ( 'NONE',  ( 1.000000000000000000, 0.000000000000000000, 0.000000000000000000 ) ) ;
#5275 = CARTESIAN_POINT ( 'NONE',  ( 9.114876806416853938, 99.49999999999998579, 19.97295714941878231 ) ) ;
#5276 = FACE_OUTER_BOUND ( 'NONE', #7053, .T. ) ;
#5277 = CARTESIAN_POINT ( 'NONE',  ( -2.256430356250000102, -2.053124999385482763, 0.000000000000000000 ) ) ;
#5278 = LINE ( 'NONE', #10095, #3119 ) ;
#5279 = CARTESIAN_POINT ( 'NONE',  ( 27.43301270000000258, 1.949999998907525178, 0.000000000000000000 ) ) ;
#5280 = ORIENTED_EDGE ( 'NONE', *, *, #2041, .T. ) ;
#5281 = PRODUCT_DEFINITION_CONTEXT ( 'detailed design', #3146, 'design' ) ;
#5282 = EDGE_CURVE ( 'NONE', #3939, #834, #7562, .T. ) ;
#5283 = CARTESIAN_POINT ( 'NONE',  ( -15.10737684033046335, 100.0000000000000000, 15.12848924955281049 ) ) ;
#5284 = FACE_OUTER_BOUND ( 'NONE', #851, .T. ) ;
#5285 = CARTESIAN_POINT ( 'NONE',  ( -27.00000000000001421, 4.249999997815050001, 11.18376618407356560 ) ) ;
#5286 = CARTESIAN_POINT ( 'NONE',  ( -11.18376618407358336, 4.549999999999999822, 26.99999999999999645 ) ) ;
#5287 = VECTOR ( 'NONE', #1384, 1000.000000000000000 ) ;
#5288 = ORIENTED_EDGE ( 'NONE', *, *, #8840, .T. ) ;
#5289 = CARTESIAN_POINT ( 'NONE',  ( -1.128215178124998497, -0.5156249993854828961, 1.954126010382872147 ) ) ;
#5290 = CARTESIAN_POINT ( 'NONE',  ( -2.500000000000000000, -4.049999999999999822, 0.000000000000000000 ) ) ;
#5291 = ORIENTED_EDGE ( 'NONE', *, *, #2238, .T. ) ;
#5292 = CARTESIAN_POINT ( 'NONE',  ( 19.39806930854668110, 2.749999998907525001, -19.39806930854668110 ) ) ;
#5293 = AXIS2_PLACEMENT_3D ( 'NONE', #2193, #3763, #2248 ) ;
#5294 = LINE ( 'NONE', #8607, #1068 ) ;
#5295 = B_SPLINE_CURVE_WITH_KNOTS ( 'NONE', 3,
 ( #8224, #271, #3567, #5822, #6601, #6806, #9894, #6024, #2730, #9843, #1212, #4199, #5918, #9064, #4350 ),
 .UNSPECIFIED., .F., .F.,
 ( 4, 1, 1, 1, 1, 1, 1, 1, 1, 1, 1, 1, 4 ),
 ( 0.000000000000000000, 0.1166921615859537187, 0.2277195327244859735, 0.3361971884410420164, 0.4453256767247914527, 0.5018483577356800396, 0.5617326728321133666, 0.6243107931132723110, 0.6909729641497043273, 0.7615676753376537933, 0.8363829297815326136, 0.9156607463298391814, 0.9999999999999998890 ),
 .UNSPECIFIED. ) ;
#5296 = CARTESIAN_POINT ( 'NONE',  ( 1.653273178848927064E-15, 1.800000000000000266, -27.00000000000000355 ) ) ;
#5297 = VECTOR ( 'NONE', #9030, 1000.000000000000000 ) ;
#5298 = CARTESIAN_POINT ( 'NONE',  ( 2.859712287474666770, 100.0000000000000000, -22.17872625191749236 ) ) ;
#5299 = EDGE_LOOP ( 'NONE', ( #4169, #595, #3893, #9829 ) ) ;
#5300 = ADVANCED_FACE ( 'NONE', ( #9924, #4955 ), #8156, .T. ) ;
#5301 = DIRECTION ( 'NONE',  ( 0.9197781680807419757, 0.000000000000000000, -0.3924386850477849520 ) ) ;
#5302 = CARTESIAN_POINT ( 'NONE',  ( -2.256430356250000102, -2.090624999385482852, -1.302750673588580321 ) ) ;
#5303 = EDGE_LOOP ( 'NONE', ( #9930, #1460, #8687, #1583 ) ) ;
#5304 = CARTESIAN_POINT ( 'NONE',  ( -22.25406130147340633, 100.0000000000000000, -9.998337329044998611 ) ) ;
#5305 = EDGE_CURVE ( 'NONE', #5423, #3612, #2446, .T. ) ;
#5306 = CARTESIAN_POINT ( 'NONE',  ( -16.01161620991261358, 100.0000000000000000, 17.10240122391520146 ) ) ;
#5307 = AXIS2_PLACEMENT_3D ( 'NONE', #6112, #2825, #5274 ) ;
#5308 = CARTESIAN_POINT ( 'NONE',  ( 4.154273145530666511, 99.50000000000000000, -22.82723029927519676 ) ) ;
#5309 = CARTESIAN_POINT ( 'NONE',  ( -1.128215178125000273, -1.228124999385483029, -1.954126010382871259 ) ) ;
#5310 = CARTESIAN_POINT ( 'NONE',  ( 3.058419780146050648, 100.0000000000000000, -23.12871267107006545 ) ) ;
#5311 = EDGE_CURVE ( 'NONE', #10148, #1877, #7113, .T. ) ;
#5312 =( BOUNDED_CURVE ( )  B_SPLINE_CURVE ( 2, ( #282, #6710, #9906, #9126, #437, #2848, #2055, #5140, #8340 ),
 .UNSPECIFIED., .F., .T. ) 
 B_SPLINE_CURVE_WITH_KNOTS ( ( 3, 2, 2, 2, 3 ),
 ( 0.7500000000000000000, 0.7678571428571429047, 0.7857142857142856984, 0.8035714285714286031, 0.8214285714285713969 ),
 .UNSPECIFIED. ) 
 CURVE ( )  GEOMETRIC_REPRESENTATION_ITEM ( )  RATIONAL_B_SPLINE_CURVE ( ( 1.000000000000000000, 0.9238795325112867385, 1.000000000000000000, 0.9238795325112867385, 1.000000000000000000, 0.9238795325112867385, 1.000000000000000000, 0.9238795325112867385, 1.000000000000000000 ) ) 
 REPRESENTATION_ITEM ( '' )  );
#5313 = B_SPLINE_CURVE_WITH_KNOTS ( 'NONE', 3,
 ( #9995, #10216, #2201, #6848, #5172, #9373, #8371, #1309, #2087, #8595, #4607, #2030, #9256, #5283, #8423 ),
 .UNSPECIFIED., .F., .F.,
 ( 4, 1, 1, 1, 1, 1, 1, 1, 1, 1, 1, 1, 4 ),
 ( 0.000000000000000000, 0.08635447908391848115, 0.1695936995346988552, 0.2509241109261274860, 0.3325843554298174576, 0.4138183564518133073, 0.4948404748415979881, 0.5772065644957810049, 0.6619893985813737336, 0.7474108716807353892, 0.8313115314839791825, 0.9147691218156368542, 1.000000000000000000 ),
 .UNSPECIFIED. ) ;
#5314 = EDGE_CURVE ( 'NONE', #7448, #7769, #8988, .T. ) ;
#5315 = VECTOR ( 'NONE', #1532, 1000.000000000000000 ) ;
#5316 = CARTESIAN_POINT ( 'NONE',  ( 5.243816414761435674, 100.0000000000000000, -23.48558366465980995 ) ) ;
#5317 = EDGE_CURVE ( 'NONE', #717, #4569, #4815, .T. ) ;
#5318 = CARTESIAN_POINT ( 'NONE',  ( -0.6698729810778081273, -2.551346188203300169, 2.499999999999999112 ) ) ;
#5319 = CARTESIAN_POINT ( 'NONE',  ( 2.500000000000000000, -2.887500000000000178, -1.443375672974065438 ) ) ;
#5320 = VERTEX_POINT ( 'NONE', #5206 ) ;
#5321 = LINE ( 'NONE', #4424, #380 ) ;
#5322 = CARTESIAN_POINT ( 'NONE',  ( -2.500000000000000000, -4.443749998770965881, 0.000000000000000000 ) ) ;
#5323 = CARTESIAN_POINT ( 'NONE',  ( -1.128215178125000273, -1.115624999385482985, -1.954126010382871259 ) ) ;
#5324 = VECTOR ( 'NONE', #2553, 1000.000000000000000 ) ;
#5325 = CARTESIAN_POINT ( 'NONE',  ( 9.910564025336874749, 99.50000000000001421, 20.75459158945058036 ) ) ;
#5326 = ORIENTED_EDGE ( 'NONE', *, *, #4474, .F. ) ;
#5327 = ADVANCED_FACE ( 'NONE', ( #8461 ), #509, .T. ) ;
#5328 = CARTESIAN_POINT ( 'NONE',  ( -0.6698729810778063509, -0.9361538093386314596, -2.500000000000000000 ) ) ;
#5329 = DIRECTION ( 'NONE',  ( 0.000000000000000000, -1.000000000000000000, 0.000000000000000000 ) ) ;
#5330 = DIRECTION ( 'NONE',  ( -1.000000000000000000, 0.000000000000000000, -0.000000000000000000 ) ) ;
#5331 = DIRECTION ( 'NONE',  ( 0.000000000000000000, 0.000000000000000000, -1.000000000000000000 ) ) ;
#5332 = ORIENTED_EDGE ( 'NONE', *, *, #9066, .T. ) ;
#5333 = CARTESIAN_POINT ( 'NONE',  ( 23.82500000000000284, 72.50000000000001421, -2.917720998968569322E-15 ) ) ;
#5334 = CARTESIAN_POINT ( 'NONE',  ( 19.39806930854668110, 2.849999998907525089, -19.39806930854668110 ) ) ;
#5335 = ORIENTED_EDGE ( 'NONE', *, *, #10165, .F. ) ;
#5336 =( REPRESENTATION_RELATIONSHIP ('NONE','NONE', #3375, #4065 ) REPRESENTATION_RELATIONSHIP_WITH_TRANSFORMATION ( #360 )SHAPE_REPRESENTATION_RELATIONSHIP( ) );
#5337 = CARTESIAN_POINT ( 'NONE',  ( -1.767625397874844694E-16, -1.462499999999999911, -2.886751345948128655 ) ) ;
#5338 = SHAPE_DEFINITION_REPRESENTATION ( #2431, #4065 ) ;
#5339 = CARTESIAN_POINT ( 'NONE',  ( -22.64023588676181475, 99.50000000000000000, -10.01165679465830927 ) ) ;
#5340 = CARTESIAN_POINT ( 'NONE',  ( 2.500000000000000444, -3.862499999999999822, 1.443375672974063439 ) ) ;
#5341 = CARTESIAN_POINT ( 'NONE',  ( -1.595409442497313560E-16, -1.715624999385482630, -2.605501347177161087 ) ) ;
#5342 = CARTESIAN_POINT ( 'NONE',  ( 19.39806930854668110, 5.149999998907524912, -19.39806930854668110 ) ) ;
#5343 = CARTESIAN_POINT ( 'NONE',  ( -27.43301270000000258, 3.099999998907525089, -11.36312591709336317 ) ) ;
#5345 = EDGE_LOOP ( 'NONE', ( #8886, #5872, #6019, #1289 ) ) ;
#5344 = ORIENTED_EDGE ( 'NONE', *, *, #3854, .T. ) ;
#5346 = CARTESIAN_POINT ( 'NONE',  ( -16.24524625128438515, 100.0000000000000284, 16.53274063862002308 ) ) ;
#5347 = CARTESIAN_POINT ( 'NONE',  ( 0.000000000000000000, -5.000000000000000000, 0.000000000000000000 ) ) ;
#5348 = LINE ( 'NONE', #3879, #9901 ) ;
#5349 = CARTESIAN_POINT ( 'NONE',  ( 0.000000000000000000, 87.00000000000001421, 0.000000000000000000 ) ) ;
#5350 = ORIENTED_EDGE ( 'NONE', *, *, #3721, .F. ) ;
#5351 = CARTESIAN_POINT ( 'NONE',  ( 2.256430356249999658, -1.678124999385482541, -1.302750673588581432 ) ) ;
#5352 = CARTESIAN_POINT ( 'NONE',  ( -22.22752541189434794, 99.49999999999994316, -11.26717589342885084 ) ) ;
#5353 = ORIENTED_EDGE ( 'NONE', *, *, #9785, .F. ) ;
#5354 = ADVANCED_FACE ( 'NONE', ( #6942 ), #1455, .T. ) ;
#5355 = DIRECTION ( 'NONE',  ( 0.000000000000000000, -0.000000000000000000, 1.000000000000000000 ) ) ;
#5356 = CARTESIAN_POINT ( 'NONE',  ( -27.43301270000000258, 3.049999998907525267, -3.359575119402369376E-15 ) ) ;
#5357 = EDGE_CURVE ( 'NONE', #229, #7425, #8271, .T. ) ;
#5358 =( LENGTH_UNIT ( ) NAMED_UNIT ( * ) SI_UNIT ( .MILLI., .METRE. ) );
#5359 = CARTESIAN_POINT ( 'NONE',  ( 0.6698729810778050187, -2.961153809338631593, 2.500000000000000444 ) ) ;
#5360 = CARTESIAN_POINT ( 'NONE',  ( -20.63200021313574695, 100.0000000000000000, -10.19493994959453431 ) ) ;
#5361 = CARTESIAN_POINT ( 'NONE',  ( 8.901217755223779449, 100.0000000000000711, 19.92336871027421097 ) ) ;
#5362 = ORIENTED_EDGE ( 'NONE', *, *, #4984, .F. ) ;
#5363 = CARTESIAN_POINT ( 'NONE',  ( -16.57330815294036697, 99.50000000000001421, 15.84440382193293217 ) ) ;
#5364 = CARTESIAN_POINT ( 'NONE',  ( 8.102924533678123709, 99.50000000000000000, 20.98904009517733726 ) ) ;
#5365 = ORIENTED_EDGE ( 'NONE', *, *, #4209, .T. ) ;
#5366 = CARTESIAN_POINT ( 'NONE',  ( -2.256430356250000102, -1.603124999385482807, 0.000000000000000000 ) ) ;
#5367 = ORIENTED_EDGE ( 'NONE', *, *, #1897, .T. ) ;
#5368 = CARTESIAN_POINT ( 'NONE',  ( 1.250000000000001110, -0.7499999999999998890, 2.165063509461096380 ) ) ;
#5369 = CARTESIAN_POINT ( 'NONE',  ( -20.97771390646102319, 99.50000000000002842, -10.03345247102482674 ) ) ;
#5370 = ADVANCED_FACE ( 'NONE', ( #4648 ), #10142, .F. ) ;
#5371 = CARTESIAN_POINT ( 'NONE',  ( 1.128215178125001161, -2.353124999385482585, 1.954126010382870815 ) ) ;
#5372 = LINE ( 'NONE', #1595, #9055 ) ;
#5373 = ORIENTED_EDGE ( 'NONE', *, *, #4110, .T. ) ;
#5374 = CARTESIAN_POINT ( 'NONE',  ( 1.653273178848927064E-15, 5.599999997815050534, -27.00000000000000355 ) ) ;
#5375 = CARTESIAN_POINT ( 'NONE',  ( 4.570993444255353921, 99.49999999999998579, -21.37574484917381668 ) ) ;
#5376 = CARTESIAN_POINT ( 'NONE',  ( -19.09188309203678813, 1.300000000000000266, 19.09188309203678457 ) ) ;
#5377 = CARTESIAN_POINT ( 'NONE',  ( -16.07368679829020763, 100.0000000000000000, 17.11560437002838952 ) ) ;
#5378 = ORIENTED_EDGE ( 'NONE', *, *, #887, .T. ) ;
#5379 = CARTESIAN_POINT ( 'NONE',  ( 2.500000000000000444, -1.162499999999999645, 1.443375672974063439 ) ) ;
#5380 = FACE_OUTER_BOUND ( 'NONE', #5299, .T. ) ;
#5381 = CARTESIAN_POINT ( 'NONE',  ( -2.256430356250000102, -0.6281249993854829405, -1.302750673588580321 ) ) ;
#5382 = EDGE_LOOP ( 'NONE', ( #7605, #588, #5942, #7823 ) ) ;
#5383 = DIRECTION ( 'NONE',  ( -0.9572638942369904314, 0.000000000000000000, 0.2892158999609669712 ) ) ;
#5384 = CARTESIAN_POINT ( 'NONE',  ( 8.465276868207817884, 100.0000000000000142, 19.66343818277063704 ) ) ;
#5385 = B_SPLINE_CURVE_WITH_KNOTS ( 'NONE', 3,
 ( #5727, #6598, #9009, #1829, #9890, #1003, #9788, #2625, #1931, #7480, #8913, #320, #7335, #5024, #8221, #3459, #269, #1736, #4246 ),
 .UNSPECIFIED., .F., .F.,
 ( 4, 1, 1, 1, 1, 1, 1, 1, 1, 1, 1, 1, 1, 1, 1, 1, 4 ),
 ( 0.000000000000000000, 0.08029080299619884009, 0.1602734547033792534, 0.2412010114815648643, 0.3246404098231062685, 0.3670482715230247162, 0.4085690013065461645, 0.4496707568484641926, 0.4905395156191099670, 0.5313644394553277417, 0.5726744073239632415, 0.6138178896263115636, 0.6555018086025313773, 0.7394546411270094266, 0.8240219501092651555, 0.9101625766452680066, 1.000000000000000000 ),
 .UNSPECIFIED. ) ;
#5386 = FACE_OUTER_BOUND ( 'NONE', #3897, .T. ) ;
#5387 = CARTESIAN_POINT ( 'NONE',  ( -16.56356094049941419, 99.49999999999997158, 15.77213757552179629 ) ) ;
#5388 = EDGE_LOOP ( 'NONE', ( #2047, #7952, #5931, #3347 ) ) ;
#5389 = CARTESIAN_POINT ( 'NONE',  ( -16.42071764973191250, 100.0000000000000142, 16.76105279315999042 ) ) ;
#5390 = VECTOR ( 'NONE', #5036, 1000.000000000000114 ) ;
#5391 = CARTESIAN_POINT ( 'NONE',  ( -27.43301270000000258, 1.549999998907525267, -3.359575119402369376E-15 ) ) ;
#5392 = CIRCLE ( 'NONE', #6553, 22.50000000000000355 ) ;
#5393 = ORIENTED_EDGE ( 'NONE', *, *, #1977, .T. ) ;
#5394 = EDGE_CURVE ( 'NONE', #872, #5320, #9314, .T. ) ;
#5395 = CARTESIAN_POINT ( 'NONE',  ( 1.249999999999999334, -3.750000000000000000, -2.165063509461096825 ) ) ;
#5396 = DIRECTION ( 'NONE',  ( 1.000000000000000000, 0.000000000000000000, 0.000000000000000000 ) ) ;
#5397 = DIRECTION ( 'NONE',  ( 0.000000000000000000, -0.000000000000000000, 1.000000000000000000 ) ) ;
#5398 = CARTESIAN_POINT ( 'NONE',  ( 2.256430356250000546, -1.865624999385482985, 1.302750673588579877 ) ) ;
#5399 = CARTESIAN_POINT ( 'NONE',  ( -16.74216497804568604, 99.50000000000001421, 15.31795814478965312 ) ) ;
#5400 = CARTESIAN_POINT ( 'NONE',  ( -11.36312591709337383, 0.8999999989075252449, 27.43301269999999548 ) ) ;
#5401 = ORIENTED_EDGE ( 'NONE', *, *, #2320, .F. ) ;
#5402 = UNCERTAINTY_MEASURE_WITH_UNIT (LENGTH_MEASURE( 1.000000000000000082E-05 ), #9623, 'distance_accuracy_value', 'NONE');
#5403 = DIRECTION ( 'NONE',  ( -0.8616861851997287269, 0.000000000000000000, 0.5074415416931677969 ) ) ;
#5404 = DIRECTION ( 'NONE',  ( 0.000000000000000000, 0.000000000000000000, -1.000000000000000000 ) ) ;
#5405 = CARTESIAN_POINT ( 'NONE',  ( 2.837666006185522782, 99.50000000000000000, -22.03040394835428373 ) ) ;
#5406 = CARTESIAN_POINT ( 'NONE',  ( 5.243816414761435674, 99.50000000000000000, -23.48558366465980995 ) ) ;
#5407 = EDGE_LOOP ( 'NONE', ( #2301, #10277, #6617, #179 ) ) ;
#5408 = CARTESIAN_POINT ( 'NONE',  ( -2.256430356250000102, -0.6281249993854829405, -1.302750673588580321 ) ) ;
#5409 = CARTESIAN_POINT ( 'NONE',  ( 4.433602057339688152, 99.50000000000000000, -21.25644978738549540 ) ) ;
#5410 = ORIENTED_EDGE ( 'NONE', *, *, #967, .T. ) ;
#5411 = CARTESIAN_POINT ( 'NONE',  ( -2.256430356250000102, -1.490624999385482763, 0.000000000000000000 ) ) ;
#5412 = CARTESIAN_POINT ( 'NONE',  ( 27.43301270000000258, 1.099999998907525089, -11.36312591709336139 ) ) ;
#5413 = PRESENTATION_LAYER_ASSIGNMENT (  '', '', ( #9740 ) ) ;
#5414 = SURFACE_STYLE_USAGE ( .BOTH. , #3009 ) ;
#5415 = CARTESIAN_POINT ( 'NONE',  ( 2.500000000000000000, -2.831249998770965615, -1.443375672974065438 ) ) ;
#5416 = AXIS2_PLACEMENT_3D ( 'NONE', #99, #6528, #935 ) ;
#5417 = DIRECTION ( 'NONE',  ( -0.000000000000000000, -1.000000000000000000, -0.000000000000000000 ) ) ;
#5418 = CARTESIAN_POINT ( 'NONE',  ( 8.540544597724410991, 100.0000000000000284, 19.98924338346217766 ) ) ;
#5419 = ORIENTED_EDGE ( 'NONE', *, *, #10119, .T. ) ;
#5420 = CARTESIAN_POINT ( 'NONE',  ( -16.45635306197508996, 99.50000000000000000, 15.51056558312563105 ) ) ;
#5421 = CARTESIAN_POINT ( 'NONE',  ( 8.187169943530866689, 99.99999999999998579, 20.27434297626003712 ) ) ;
#5422 = COLOUR_RGB ( '',0.8941176470588234615, 0.8941176470588234615, 0.8941176470588234615 ) ;
#5423 = VERTEX_POINT ( 'NONE', #5264 ) ;
#5424 = CARTESIAN_POINT ( 'NONE',  ( -2.256430356250000102, -3.890624999385482674, -1.302750673588580321 ) ) ;
#5425 = ORIENTED_EDGE ( 'NONE', *, *, #5787, .T. ) ;
#5426 = B_SPLINE_CURVE_WITH_KNOTS ( 'NONE', 3,
 ( #2697, #8243, #2646, #5788, #5939, #8982, #5836, #4266, #5745, #339, #8195, #9132, #5147, #1175, #1071, #9914, #3377, #6524, #4949 ),
 .UNSPECIFIED., .F., .F.,
 ( 4, 1, 1, 1, 1, 1, 1, 1, 1, 1, 1, 1, 1, 1, 1, 1, 4 ),
 ( 0.000000000000000000, 0.06463354665699841406, 0.1274839167070160040, 0.1893660780973640267, 0.2502738481868047038, 0.3108090901939400408, 0.3728692346228669741, 0.4358265942208103261, 0.5002515515682643965, 0.5647461136436963125, 0.6273730017603231790, 0.6892793264321037672, 0.7497280364991398827, 0.8111249352628771003, 0.8723480300361200479, 0.9354359082354426480, 1.000000000000000000 ),
 .UNSPECIFIED. ) ;
#5427 = CARTESIAN_POINT ( 'NONE',  ( -15.34367147589386349, 100.0000000000000426, 16.87599331055909602 ) ) ;
#5428 = CARTESIAN_POINT ( 'NONE',  ( -21.24882413972086681, 99.50000000000002842, -9.742484589929601313 ) ) ;
#5429 = CARTESIAN_POINT ( 'NONE',  ( -1.595409442497313560E-16, -0.3656249993854829294, -2.605501347177161087 ) ) ;
#5430 = CARTESIAN_POINT ( 'NONE',  ( 5.142436925601051811, 99.49999999999995737, -24.04117066426968563 ) ) ;
#5431 = FACE_BOUND ( 'NONE', #4503, .T. ) ;
#5432 = EDGE_CURVE ( 'NONE', #7437, #229, #9764, .T. ) ;
#5433 = CARTESIAN_POINT ( 'NONE',  ( -1.250000000000000222, -1.818749998770965881, -2.165063509461096825 ) ) ;
#5434 = ORIENTED_EDGE ( 'NONE', *, *, #8411, .F. ) ;
#5435 = CARTESIAN_POINT ( 'NONE',  ( 3.124251205490514494, 99.50000000000000000, -23.02140944421609703 ) ) ;
#5436 = FACE_BOUND ( 'NONE', #9392, .T. ) ;
#5437 = ORIENTED_EDGE ( 'NONE', *, *, #9704, .T. ) ;
#5438 = CARTESIAN_POINT ( 'NONE',  ( 3.061616997868383141E-16, 0.000000000000000000, 2.500000000000000000 ) ) ;
#5439 = CARTESIAN_POINT ( 'NONE',  ( -1.128215178124998497, -2.765624999385482674, 1.954126010382872147 ) ) ;
#5440 = CARTESIAN_POINT ( 'NONE',  ( -21.79396932678589849, 100.0000000000000000, -9.306975108219608828 ) ) ;
#5441 = CARTESIAN_POINT ( 'NONE',  ( 4.331079892889020400, 99.50000000000000000, -24.67336562508343079 ) ) ;
#5442 = EDGE_CURVE ( 'NONE', #6092, #498, #3702, .T. ) ;
#5443 = CARTESIAN_POINT ( 'NONE',  ( -22.28244091826395135, 100.0000000000000000, -10.68852969318427881 ) ) ;
#5444 = ORIENTED_EDGE ( 'NONE', *, *, #3465, .T. ) ;
#5445 = CARTESIAN_POINT ( 'NONE',  ( -15.49723655759404295, 99.49999999999997158, 15.26389171799780264 ) ) ;
#5446 = CARTESIAN_POINT ( 'NONE',  ( 1.679787559701184688E-15, 1.349999998907525312, -27.43301270000000258 ) ) ;
#5447 = ORIENTED_EDGE ( 'NONE', *, *, #181, .F. ) ;
#5448 = CARTESIAN_POINT ( 'NONE',  ( -0.7756784236033643642, -5.052895385698252362, -2.964907715781667452 ) ) ;
#5449 = EDGE_CURVE ( 'NONE', #10235, #4631, #7853, .T. ) ;
#5450 = VECTOR ( 'NONE', #5975, 1000.000000000000000 ) ;
#5451 = CARTESIAN_POINT ( 'NONE',  ( -8.673617379884035472E-16, -15.00000000000000000, 3.464101615137756163 ) ) ;
#5452 = CARTESIAN_POINT ( 'NONE',  ( 4.786228327491941173E-16, -1.040624999385482585, 2.605501347177161087 ) ) ;
#5453 = ADVANCED_FACE ( 'NONE', ( #10201 ), #9411, .T. ) ;
#5454 = CARTESIAN_POINT ( 'NONE',  ( 4.739008722453744049, 99.50000000000001421, -24.06821587619827696 ) ) ;
#5455 = CARTESIAN_POINT ( 'NONE',  ( -27.43301270000000969, 3.199999998907525178, 11.36312591709335429 ) ) ;
#5456 = EDGE_LOOP ( 'NONE', ( #9337, #4253, #7844, #922 ) ) ;
#5457 = EDGE_CURVE ( 'NONE', #4647, #4294, #6160, .T. ) ;
#5458 = CARTESIAN_POINT ( 'NONE',  ( -15.22739782325755442, 99.49999999999998579, 15.50750051783781025 ) ) ;
#5459 = CARTESIAN_POINT ( 'NONE',  ( -1.250000000000000222, -3.168749998770965526, -2.165063509461096825 ) ) ;
#5460 = CARTESIAN_POINT ( 'NONE',  ( 9.877377282685029372E-16, -1.181249998770965703, 2.500000000000000000 ) ) ;
#5461 = LINE ( 'NONE', #8650, #4931 ) ;
#5462 = CARTESIAN_POINT ( 'NONE',  ( -2.256430356250000102, -1.528124999385482852, -1.302750673588580321 ) ) ;
#5463 = CARTESIAN_POINT ( 'NONE',  ( 4.691018317478480526, 99.99999999999995737, -21.52316599815148024 ) ) ;
#5464 = CARTESIAN_POINT ( 'NONE',  ( 2.256430356250000546, -2.653124999385482852, 1.302750673588579877 ) ) ;
#5465 = CIRCLE ( 'NONE', #3783, 23.99999999999999645 ) ;
#5466 = CARTESIAN_POINT ( 'NONE',  ( -19.39806930854667755, 2.149999998907525356, -19.39806930854668110 ) ) ;
#5467 = PRESENTATION_STYLE_ASSIGNMENT (( #9638 ) ) ;
#5468 = DIRECTION ( 'NONE',  ( -0.000000000000000000, -1.000000000000000000, 0.000000000000000000 ) ) ;
#5469 = CARTESIAN_POINT ( 'NONE',  ( 19.09188309203678102, 1.500000000000000000, 19.09188309203678813 ) ) ;
#5470 = CARTESIAN_POINT ( 'NONE',  ( 9.044794778432494908, 100.0000000000000426, 19.94873160813952140 ) ) ;
#5471 = VERTEX_POINT ( 'NONE', #829 ) ;
#5472 = CARTESIAN_POINT ( 'NONE',  ( -16.45391695211397831, 99.50000000000004263, 16.32580124622701589 ) ) ;
#5473 = DIRECTION ( 'NONE',  ( 0.000000000000000000, 0.000000000000000000, -1.000000000000000000 ) ) ;
#5474 = CARTESIAN_POINT ( 'NONE',  ( -1.128215178125000273, -4.378124999385482496, -1.954126010382871259 ) ) ;
#5475 = ORIENTED_EDGE ( 'NONE', *, *, #4900, .F. ) ;
#5476 = ORIENTED_EDGE ( 'NONE', *, *, #9469, .T. ) ;
#5477 = CARTESIAN_POINT ( 'NONE',  ( -11.36312591709335962, 3.699999998907525622, -27.43301270000000258 ) ) ;
#5478 = CARTESIAN_POINT ( 'NONE',  ( -3.486133158594716510E-16, -4.106249998770965526, -2.500000000000000000 ) ) ;
#5479 = VECTOR ( 'NONE', #5148, 1000.000000000000000 ) ;
#5480 = CARTESIAN_POINT ( 'NONE',  ( 1.128215178125001161, -1.003124999385482718, 1.954126010382870815 ) ) ;
#5481 = SHAPE_REPRESENTATION ( 'time set dial', ( #5055 ), #1396 ) ;
#5482 = CARTESIAN_POINT ( 'NONE',  ( 4.850954546176396320, 100.0000000000000142, -24.43907202982397209 ) ) ;
#5483 = ORIENTED_EDGE ( 'NONE', *, *, #4438, .T. ) ;
#5484 = CARTESIAN_POINT ( 'NONE',  ( -2.500000000000000000, -1.837499999999999911, -1.443375672974064106 ) ) ;
#5485 = CARTESIAN_POINT ( 'NONE',  ( -1.249999999999998224, -3.018749998770965615, 2.165063509461097713 ) ) ;
#5486 = CARTESIAN_POINT ( 'NONE',  ( 4.232798786556307036, 99.50000000000000000, -24.34936571594186105 ) ) ;
#5487 = LINE ( 'NONE', #8879, #8970 ) ;
#5488 = ORIENTED_EDGE ( 'NONE', *, *, #5630, .T. ) ;
#5489 = CARTESIAN_POINT ( 'NONE',  ( -16.33590634957226229, 99.50000000000000000, 16.80570853669505382 ) ) ;
#5490 = CARTESIAN_POINT ( 'NONE',  ( -2.256430356250000102, -1.978124999385482807, -1.302750673588580321 ) ) ;
#5491 = EDGE_CURVE ( 'NONE', #4746, #4835, #3280, .T. ) ;
#5492 = ORIENTED_EDGE ( 'NONE', *, *, #4682, .F. ) ;
#5493 = CARTESIAN_POINT ( 'NONE',  ( 4.295198626299898237, 99.50000000000001421, -24.68029520312135361 ) ) ;
#5494 = CARTESIAN_POINT ( 'NONE',  ( 9.725694684612619767, 100.0000000000000000, 20.03234812723199454 ) ) ;
#5495 = CARTESIAN_POINT ( 'NONE',  ( -16.37547766376588854, 99.50000000000000000, 16.41943072543956816 ) ) ;
#5496 = ORIENTED_EDGE ( 'NONE', *, *, #4254, .F. ) ;
#5497 = CARTESIAN_POINT ( 'NONE',  ( -15.03933290382598820, 99.50000000000000000, 15.19633946010233849 ) ) ;
#5498 = CARTESIAN_POINT ( 'NONE',  ( 27.43301270000000258, 5.199999998907525622, -11.36312591709336139 ) ) ;
#5499 = EDGE_LOOP ( 'NONE', ( #5673, #8460 ) ) ;
#5500 = CIRCLE ( 'NONE', #8674, 7.500000000000000000 ) ;
#5501 = CARTESIAN_POINT ( 'NONE',  ( -2.499999999999999556, -4.012499999999999289, 1.443375672974065882 ) ) ;
#5502 = ADVANCED_FACE ( 'NONE', ( #777, #6272 ), #7946, .T. ) ;
#5503 = EDGE_CURVE ( 'NONE', #5726, #6080, #7102, .T. ) ;
#5504 = CONTEXT_DEPENDENT_SHAPE_REPRESENTATION ( #5260, #8032 ) ;
#5505 = CARTESIAN_POINT ( 'NONE',  ( 3.269123371500344710, 99.50000000000001421, -23.64665713169964434 ) ) ;
#5506 = CARTESIAN_POINT ( 'NONE',  ( 4.786228327491941173E-16, -4.190624999385482496, 2.605501347177161087 ) ) ;
#5507 = CARTESIAN_POINT ( 'NONE',  ( -16.85368146453285831, 99.49999999999998579, 16.27421966797335529 ) ) ;
#5508 = CARTESIAN_POINT ( 'NONE',  ( -27.43301270000000258, 3.949999998907525178, -3.359575119402369376E-15 ) ) ;
#5509 = CARTESIAN_POINT ( 'NONE',  ( -15.30604604128650692, 99.50000000000000000, 15.41317891555018349 ) ) ;
#5510 = CARTESIAN_POINT ( 'NONE',  ( 3.735769352376668184, 99.99999999999998579, -24.30643046864489420 ) ) ;
#5511 = CARTESIAN_POINT ( 'NONE',  ( 2.852289972453743161, 99.50000000000000000, -22.14293542748032451 ) ) ;
#5512 = CARTESIAN_POINT ( 'NONE',  ( -22.64023588676181475, 100.0000000000000000, -10.01165679465830927 ) ) ;
#5513 = CARTESIAN_POINT ( 'NONE',  ( 1.128215178124999607, -2.990624999385482763, -1.954126010382871259 ) ) ;
#5514 = CARTESIAN_POINT ( 'NONE',  ( 4.633286773149219329, 99.50000000000002842, -21.44575434969419447 ) ) ;
#5515 = VERTEX_POINT ( 'NONE', #5493 ) ;
#5516 = CARTESIAN_POINT ( 'NONE',  ( 1.128215178124999607, -2.990624999385482763, -1.954126010382871259 ) ) ;
#5517 = CARTESIAN_POINT ( 'NONE',  ( -11.36312591709337383, 3.999999998907525889, 27.43301269999999548 ) ) ;
#5518 = B_SPLINE_CURVE_WITH_KNOTS ( 'NONE', 3,
 ( #8394, #334, #235, #1996, #8237, #5833, #9079, #5195, #6711, #8190, #5141, #2641, #8341, #9025, #5880, #2797, #5783, #2742, #6765 ),
 .UNSPECIFIED., .F., .F.,
 ( 4, 1, 1, 1, 1, 1, 1, 1, 1, 1, 1, 1, 1, 1, 1, 1, 4 ),
 ( 0.000000000000000000, 0.06473908249738200005, 0.1274869542813800993, 0.1888754624962200035, 0.2498352098569301405, 0.3101749858420705941, 0.3718734486855839183, 0.4342313324889700565, 0.4990836447755341299, 0.5639614065304963120, 0.6264045329497629488, 0.6882484937299673255, 0.7493615009078817835, 0.8100377551054726011, 0.8717391907241844873, 0.9348513958286107650, 1.000000000000000000 ),
 .UNSPECIFIED. ) ;
#5519 = CARTESIAN_POINT ( 'NONE',  ( 0.000000000000000000, 70.00000000000000000, 0.000000000000000000 ) ) ;
#5520 = CARTESIAN_POINT ( 'NONE',  ( 26.99999999999999645, 0.7500000000000001110, 11.18376618407358691 ) ) ;
#5521 = CARTESIAN_POINT ( 'NONE',  ( 9.304660012616079001, 99.50000000000000000, 20.07619068507570859 ) ) ;
#5522 = PLANE ( 'NONE',  #464 ) ;
#5523 = CARTESIAN_POINT ( 'NONE',  ( -15.31787750341841559, 100.0000000000000000, 16.43551622900274722 ) ) ;
#5524 = VERTEX_POINT ( 'NONE', #9520 ) ;
#5525 = CARTESIAN_POINT ( 'NONE',  ( 2.256430356250000546, -5.015624999385482674, 1.302750673588579877 ) ) ;
#5526 = EDGE_LOOP ( 'NONE', ( #6245, #490 ) ) ;
#5527 = CARTESIAN_POINT ( 'NONE',  ( 27.43301270000000258, 3.499999998907525445, -11.36312591709336139 ) ) ;
#5528 = CARTESIAN_POINT ( 'NONE',  ( 3.824506687597884369, 99.50000000000002842, -24.68145443631992109 ) ) ;
#5529 = B_SPLINE_SURFACE_WITH_KNOTS ( 'NONE', 3, 1, ( 
 ( #3040, #461 ),
 ( #9242, #2984 ),
 ( #1406, #5389 ),
 ( #4597, #4434 ),
 ( #2869, #5270 ),
 ( #7001, #6838 ),
 ( #2247, #1295 ) ),
 .UNSPECIFIED., .F., .F., .F.,
 ( 4, 1, 1, 1, 4 ),
 ( 2, 2 ),
 ( 0.000000000000000000, 0.2687002788711734813, 0.5225003893189538173, 0.7676814173175746658, 1.000000000000000000 ),
 ( 0.000000000000000000, 1.000000000000000000 ),
 .UNSPECIFIED. ) ;
#5530 = EDGE_CURVE ( 'NONE', #6493, #6757, #10126, .T. ) ;
#5531 = CARTESIAN_POINT ( 'NONE',  ( -2.256430356249998770, -2.465624999385482852, 1.302750673588581876 ) ) ;
#5532 = CARTESIAN_POINT ( 'NONE',  ( -16.56313167360273297, 100.0000000000000284, 16.06491815633068398 ) ) ;
#5533 = DIRECTION ( 'NONE',  ( -0.9985534407235125975, 0.000000000000000000, 0.05376826219280737146 ) ) ;
#5534 = DIRECTION ( 'NONE',  ( 0.000000000000000000, -1.000000000000000000, 0.000000000000000000 ) ) ;
#5535 = ORIENTED_EDGE ( 'NONE', *, *, #9672, .F. ) ;
#5536 = CARTESIAN_POINT ( 'NONE',  ( -1.250000000000000222, -2.268749998770965615, -2.165063509461096825 ) ) ;
#5537 = CIRCLE ( 'NONE', #8039, 17.50000000000000355 ) ;
#5538 = CARTESIAN_POINT ( 'NONE',  ( 4.820889542125314620, 99.99999999999998579, -21.76289454767624676 ) ) ;
#5539 = CARTESIAN_POINT ( 'NONE',  ( -15.15193744131588183, 100.0000000000000142, 16.74589488344418697 ) ) ;
#5540 = CARTESIAN_POINT ( 'NONE',  ( 8.644881627383616873, 99.49999999999995737, 19.60534525227960145 ) ) ;
#5541 = CARTESIAN_POINT ( 'NONE',  ( -1.128215178125000273, -4.715624999385481964, -1.954126010382871259 ) ) ;
#5542 = ORIENTED_EDGE ( 'NONE', *, *, #2183, .F. ) ;
#5543 = CARTESIAN_POINT ( 'NONE',  ( -22.12191435419165941, 100.0000000000000142, -9.834338183724410598 ) ) ;
#5544 = SURFACE_STYLE_USAGE ( .BOTH. , #7998 ) ;
#5545 = CARTESIAN_POINT ( 'NONE',  ( -0.6698729810778054627, -3.451346188203299192, 2.500000000000000000 ) ) ;
#5546 = CARTESIAN_POINT ( 'NONE',  ( -16.36254897777739004, 99.50000000000001421, 15.39785597259249350 ) ) ;
#5547 = CARTESIAN_POINT ( 'NONE',  ( -19.39806930854667755, 3.849999998907525089, -19.39806930854668110 ) ) ;
#5548 = ORIENTED_EDGE ( 'NONE', *, *, #2500, .F. ) ;
#5549 = CARTESIAN_POINT ( 'NONE',  ( 2.500000000000000000, -3.374999999999999556, -3.061616997868383141E-16 ) ) ;
#5550 = CARTESIAN_POINT ( 'NONE',  ( -21.07742585509981126, 99.99999999999998579, -10.85999754779651383 ) ) ;
#5551 = CARTESIAN_POINT ( 'NONE',  ( -2.256430356250000102, -4.340624999385482852, -1.302750673588580321 ) ) ;
#5552 = CARTESIAN_POINT ( 'NONE',  ( -20.52076770522338833, 99.50000000000000000, -10.69798695537560462 ) ) ;
#5553 = CARTESIAN_POINT ( 'NONE',  ( 19.39806930854668110, 5.249999998907525445, -19.39806930854668110 ) ) ;
#5554 = CARTESIAN_POINT ( 'NONE',  ( -15.15623813234777018, 99.99999999999997158, 16.19783826294960249 ) ) ;
#5555 = CARTESIAN_POINT ( 'NONE',  ( 19.09188309203678102, 3.699999997815051067, 19.09188309203678813 ) ) ;
#5556 = CARTESIAN_POINT ( 'NONE',  ( 2.955068081869620666, 99.49999999999998579, -21.57801138750623338 ) ) ;
#5557 = EDGE_CURVE ( 'NONE', #4730, #7160, #8832, .T. ) ;
#5558 = CARTESIAN_POINT ( 'NONE',  ( 19.09188309203678813, 4.100000000000000533, -19.09188309203678813 ) ) ;
#5559 = CARTESIAN_POINT ( 'NONE',  ( 1.128215178124999607, -2.540624999385482585, -1.954126010382871259 ) ) ;
#5560 = CARTESIAN_POINT ( 'NONE',  ( 3.681717055787076642, 99.50000000000000000, -21.09125273517263111 ) ) ;
#5561 = ORIENTED_EDGE ( 'NONE', *, *, #699, .T. ) ;
#5562 = CARTESIAN_POINT ( 'NONE',  ( -2.256430356250000102, -1.528124999385482630, -1.302750673588580321 ) ) ;
#5563 = CARTESIAN_POINT ( 'NONE',  ( -19.39806930854668465, 0.8499999989075252005, 19.39806930854667755 ) ) ;
#5564 = SURFACE_SIDE_STYLE ('',( #1480 ) ) ;
#5565 = DIRECTION ( 'NONE',  ( 0.000000000000000000, -1.000000000000000000, 0.000000000000000000 ) ) ;
#5566 = TOROIDAL_SURFACE ( 'NONE', #2040, 23.82500000000000284, 1.324999999999999956 ) ;
#5567 = CARTESIAN_POINT ( 'NONE',  ( -27.00000000000000355, 3.600000000000000533, -3.306546357697854128E-15 ) ) ;
#5568 = CARTESIAN_POINT ( 'NONE',  ( 3.373335371007685435, 100.0000000000000000, -22.75111425220066863 ) ) ;
#5569 = EDGE_LOOP ( 'NONE', ( #8389, #4629, #6457, #6430 ) ) ;
#5570 = EDGE_LOOP ( 'NONE', ( #3719, #4114, #5496, #1432 ) ) ;
#5571 = CARTESIAN_POINT ( 'NONE',  ( -2.500000000000000000, 0.000000000000000000, 0.000000000000000000 ) ) ;
#5572 = CARTESIAN_POINT ( 'NONE',  ( -15.49014769301379069, 99.49999999999997158, 16.56834637662448273 ) ) ;
#5573 = ORIENTED_EDGE ( 'NONE', *, *, #6738, .F. ) ;
#5574 = CARTESIAN_POINT ( 'NONE',  ( -1.728532663107115397, -5.253648270121824559, -1.450397457657151001 ) ) ;
#5575 = ORIENTED_EDGE ( 'NONE', *, *, #8116, .T. ) ;
#5576 = COLOUR_RGB ( '',0.8941176470588234615, 0.8941176470588234615, 0.8941176470588234615 ) ;
#5577 = CARTESIAN_POINT ( 'NONE',  ( -27.43301270000000969, 1.499999998907525445, 11.36312591709335784 ) ) ;
#5578 = CARTESIAN_POINT ( 'NONE',  ( 1.653273178848927064E-15, 1.800000000000000266, -27.00000000000000355 ) ) ;
#5579 = CARTESIAN_POINT ( 'NONE',  ( -21.84904385032055174, 99.49999999999998579, -11.42736543092427404 ) ) ;
#5580 = CARTESIAN_POINT ( 'NONE',  ( 2.256430356249999658, -2.690624999385482941, -1.302750673588581432 ) ) ;
#5581 = FACE_OUTER_BOUND ( 'NONE', #5388, .T. ) ;
#5582 = CARTESIAN_POINT ( 'NONE',  ( -16.85368146453285831, 99.49999999999998579, 16.27421966797335529 ) ) ;
#5583 = CARTESIAN_POINT ( 'NONE',  ( 8.117007248954752896, 100.0000000000000142, 20.40979824468519155 ) ) ;
#5584 = EDGE_CURVE ( 'NONE', #6241, #3123, #6184, .T. ) ;
#5585 = AXIS2_PLACEMENT_3D ( 'NONE', #2781, #2154, #10111 ) ;
#5586 = EDGE_CURVE ( 'NONE', #6302, #533, #3213, .T. ) ;
#5587 = CARTESIAN_POINT ( 'NONE',  ( -2.500000000000000000, -1.331249998770965615, -1.443375672974064106 ) ) ;
#5588 = ORIENTED_EDGE ( 'NONE', *, *, #10255, .T. ) ;
#5589 = CARTESIAN_POINT ( 'NONE',  ( 4.311343222282856047, 100.0000000000000142, -24.33387958695581688 ) ) ;
#5590 = DIRECTION ( 'NONE',  ( 0.000000000000000000, 1.000000000000000000, 0.000000000000000000 ) ) ;
#5591 = CARTESIAN_POINT ( 'NONE',  ( -14.78677372028383097, 99.99999999999998579, 15.63810349997947569 ) ) ;
#5592 = CARTESIAN_POINT ( 'NONE',  ( 4.786228327491941173E-16, -4.078124999385482674, 2.605501347177161087 ) ) ;
#5593 = CARTESIAN_POINT ( 'NONE',  ( 2.936358689207804851, 99.50000000000000000, -23.74786164940363875 ) ) ;
#5594 = DIRECTION ( 'NONE',  ( 0.000000000000000000, 0.9949358851208914833, -0.1005116137503925394 ) ) ;
#5595 = CARTESIAN_POINT ( 'NONE',  ( -22.17094027205346052, 99.50000000000001421, -9.884352203306939089 ) ) ;
#5596 = DIRECTION ( 'NONE',  ( -0.2149789550291109352, 0.000000000000000000, -0.9766186814179788067 ) ) ;
#5597 = CARTESIAN_POINT ( 'NONE',  ( 11.36312591709336850, 4.199999998907525622, 27.43301269999999903 ) ) ;
#5598 = EDGE_LOOP ( 'NONE', ( #6608, #2156, #4161, #8077 ) ) ;
#5599 = CARTESIAN_POINT ( 'NONE',  ( 1.250000000000001110, -3.899999999999999911, 2.165063509461096380 ) ) ;
#5600 = VECTOR ( 'NONE', #7228, 1000.000000000000000 ) ;
#5601 = CARTESIAN_POINT ( 'NONE',  ( 3.328702480760086235, 99.49999999999997158, -23.35145716610488975 ) ) ;
#5602 = CARTESIAN_POINT ( 'NONE',  ( 4.786228327491941173E-16, -5.090624999385482852, 2.605501347177161087 ) ) ;
#5603 = CARTESIAN_POINT ( 'NONE',  ( -20.96129225301843135, 99.50000000000001421, -10.68089388303413934 ) ) ;
#5604 = CARTESIAN_POINT ( 'NONE',  ( -11.36312591709335962, 4.599999998907525978, -27.43301270000000258 ) ) ;
#5605 = CARTESIAN_POINT ( 'NONE',  ( -15.30066472929571653, 99.49999999999998579, 16.41738810589640707 ) ) ;
#5606 = PLANE ( 'NONE',  #9815 ) ;
#5607 = CARTESIAN_POINT ( 'NONE',  ( -15.42956291708403782, 99.49999999999998579, 16.53061251458192515 ) ) ;
#5608 = B_SPLINE_SURFACE_WITH_KNOTS ( 'NONE', 3, 1, ( 
 ( #1146, #3447 ),
 ( #4337, #6636 ),
 ( #9832, #6588 ),
 ( #3499, #2570 ),
 ( #5810, #2615 ),
 ( #2772, #5169 ),
 ( #5064, #6685 ),
 ( #9779, #7521 ),
 ( #9938, #2664 ),
 ( #8953, #5856 ),
 ( #9001, #362 ) ),
 .UNSPECIFIED., .F., .F., .F.,
 ( 4, 1, 1, 1, 1, 1, 1, 1, 4 ),
 ( 2, 2 ),
 ( 0.000000000000000000, 0.1307887167449866828, 0.2576322083635017579, 0.3824781763252146916, 0.5056045358258490774, 0.6278910088851102911, 0.7502354365656509483, 0.8735741898580190457, 1.000000000000000000 ),
 ( 0.000000000000000000, 1.000000000000000000 ),
 .UNSPECIFIED. ) ;
#5609 = CARTESIAN_POINT ( 'NONE',  ( -22.43208371148383762, 100.0000000000000000, -9.654966607469265938 ) ) ;
#5610 = CARTESIAN_POINT ( 'NONE',  ( 4.786228327491940187E-16, -4.528124999385482852, 2.605501347177161087 ) ) ;
#5611 = CARTESIAN_POINT ( 'NONE',  ( 4.358720771404392735, 100.0000000000000000, -21.20742720589606378 ) ) ;
#5612 = AXIS2_PLACEMENT_3D ( 'NONE', #2614, #5855, #2770 ) ;
#5613 = ORIENTED_EDGE ( 'NONE', *, *, #3853, .T. ) ;
#5614 = CARTESIAN_POINT ( 'NONE',  ( -1.128215178125000273, -2.915624999385482585, -1.954126010382871259 ) ) ;
#5615 = CARTESIAN_POINT ( 'NONE',  ( 11.36312591709336850, 0.9999999989075254447, 27.43301269999999903 ) ) ;
#5616 = CARTESIAN_POINT ( 'NONE',  ( -16.49882833452567965, 99.50000000000000000, 15.05677840364783115 ) ) ;
#5617 = EDGE_CURVE ( 'NONE', #3111, #1260, #4799, .T. ) ;
#5618 = CARTESIAN_POINT ( 'NONE',  ( 19.39806930854668110, 0.3499999989075252560, -19.39806930854668110 ) ) ;
#5619 = CARTESIAN_POINT ( 'NONE',  ( 0.000000000000000000, 75.00000000000001421, 0.000000000000000000 ) ) ;
#5620 = AXIS2_PLACEMENT_3D ( 'NONE', #2998, #5403, #528 ) ;
#5621 = FACE_OUTER_BOUND ( 'NONE', #2438, .T. ) ;
#5622 = CARTESIAN_POINT ( 'NONE',  ( 19.09188309203678102, 2.099999997815050090, 19.09188309203678813 ) ) ;
#5623 = AXIS2_PLACEMENT_3D ( 'NONE', #6202, #1496, #7934 ) ;
#5624 = CARTESIAN_POINT ( 'NONE',  ( 1.128215178125001161, -4.603124999385482141, 1.954126010382870815 ) ) ;
#5625 = CARTESIAN_POINT ( 'NONE',  ( 27.43301269999999548, 2.599999998907525089, 11.36312591709337916 ) ) ;
#5626 = CARTESIAN_POINT ( 'NONE',  ( 4.295198626299898237, 100.0000000000000142, -24.68029520312135361 ) ) ;
#5627 = DIRECTION ( 'NONE',  ( 0.9197781680807419757, 0.000000000000000000, -0.3924386850477849520 ) ) ;
#5628 = CARTESIAN_POINT ( 'NONE',  ( 2.256430356250000102, -4.978124999385482141, -2.763330213280484622E-16 ) ) ;
#5629 = DIRECTION ( 'NONE',  ( -0.000000000000000000, -1.000000000000000000, -0.000000000000000000 ) ) ;
#5630 = EDGE_CURVE ( 'NONE', #834, #1366, #7374, .T. ) ;
#5631 = CARTESIAN_POINT ( 'NONE',  ( -16.90689012439429462, 99.99999999999998579, 16.08742389234230785 ) ) ;
#5632 = CARTESIAN_POINT ( 'NONE',  ( 5.243816414761435674, 100.0000000000000000, -23.48558366465980995 ) ) ;
#5633 = EDGE_CURVE ( 'NONE', #4987, #717, #6450, .T. ) ;
#5634 = CARTESIAN_POINT ( 'NONE',  ( 5.302876193624534821E-16, -1.631249998770965881, 2.886751345948128655 ) ) ;
#5635 = AXIS2_PLACEMENT_3D ( 'NONE', #1262, #9889, #7638 ) ;
#5636 = CARTESIAN_POINT ( 'NONE',  ( 4.232798786556307036, 100.0000000000000142, -24.34936571594186105 ) ) ;
#5637 = LINE ( 'NONE', #7302, #4791 ) ;
#5638 = EDGE_CURVE ( 'NONE', #2588, #9675, #9735, .T. ) ;
#5639 = CARTESIAN_POINT ( 'NONE',  ( -15.03933290382598820, 100.0000000000000000, 15.19633946010233849 ) ) ;
#5640 = CARTESIAN_POINT ( 'NONE',  ( -1.128215178124998497, -3.665624999385482585, 1.954126010382872147 ) ) ;
#5641 = EDGE_CURVE ( 'NONE', #647, #7160, #5859, .T. ) ;
#5642 = VECTOR ( 'NONE', #782, 1000.000000000000000 ) ;
#5643 = ORIENTED_EDGE ( 'NONE', *, *, #1450, .T. ) ;
#5644 = DIRECTION ( 'NONE',  ( 0.000000000000000000, -1.000000000000000000, 0.000000000000000000 ) ) ;
#5645 = VECTOR ( 'NONE', #4307, 1000.000000000000000 ) ;
#5646 = EDGE_CURVE ( 'NONE', #1777, #7350, #7331, .T. ) ;
#5647 = CARTESIAN_POINT ( 'NONE',  ( -22.06741020400400188, 99.50000000000004263, -9.788922322134999021 ) ) ;
#5648 = CARTESIAN_POINT ( 'NONE',  ( 0.000000000000000000, -20.00000000000000000, -2.500000000000000444 ) ) ;
#5649 = CARTESIAN_POINT ( 'NONE',  ( 9.114876806416853938, 99.99999999999998579, 19.97295714941878231 ) ) ;
#5650 = VERTEX_POINT ( 'NONE', #6745 ) ;
#5651 = CARTESIAN_POINT ( 'NONE',  ( 4.405197143102897783, 99.49999999999995737, -21.72932741277565682 ) ) ;
#5652 = EDGE_CURVE ( 'NONE', #9254, #2231, #2721, .T. ) ;
#5653 = CARTESIAN_POINT ( 'NONE',  ( 3.659868213429061878, 100.0000000000000000, -22.50687739797974274 ) ) ;
#5654 = CARTESIAN_POINT ( 'NONE',  ( 4.786228327491941173E-16, -4.640624999385482674, 2.605501347177161087 ) ) ;
#5655 = CARTESIAN_POINT ( 'NONE',  ( 27.00000000000000355, 2.249999997815050445, -11.18376618407356737 ) ) ;
#5656 =( BOUNDED_CURVE ( )  B_SPLINE_CURVE ( 2, ( #159, #7466, #1141, #3440, #6582, #990, #2612, #9773, #9151 ),
 .UNSPECIFIED., .F., .F. ) 
 B_SPLINE_CURVE_WITH_KNOTS ( ( 3, 2, 2, 2, 3 ),
 ( 0.8541666666666667407, 0.8611111111111111605, 0.8750000000000000000, 0.8888888888888888395, 0.8958333333333333703 ),
 .UNSPECIFIED. ) 
 CURVE ( )  GEOMETRIC_REPRESENTATION_ITEM ( )  RATIONAL_B_SPLINE_CURVE ( ( 0.9330127018922192983, 0.9330127018922198534, 1.000000000000000000, 0.8660254037844387076, 1.000000000000000000, 0.8660254037844387076, 1.000000000000000000, 0.9330127018922187432, 0.9330127018922192983 ) ) 
 REPRESENTATION_ITEM ( '' )  );
#5657 = CARTESIAN_POINT ( 'NONE',  ( 5.725936192474917696, 99.50000000000000000, 21.08018326417248645 ) ) ;
#5658 = B_SPLINE_CURVE_WITH_KNOTS ( 'NONE', 3,
 ( #6391, #2415, #8800, #4268, #111, #392, #3303, #288, #1899, #9082, #2000, #9970, #6443, #9180, #6718, #6492, #1072, #7222, #9915 ),
 .UNSPECIFIED., .F., .F.,
 ( 4, 1, 1, 1, 1, 1, 1, 1, 1, 1, 1, 1, 1, 1, 1, 1, 4 ),
 ( 0.000000000000000000, 0.07313710028058939550, 0.1429478298248799129, 0.2105045057187734658, 0.2751999312753631854, 0.3390602298032547868, 0.4018764873508149926, 0.4650016082884899093, 0.5281538368899733049, 0.5906348070863262079, 0.6510495490485337378, 0.7103018853965116230, 0.7674338915725752441, 0.8249350906448947862, 0.8823686014076175255, 0.9405824579944982444, 1.000000000000000000 ),
 .UNSPECIFIED. ) ;
#5659 = CARTESIAN_POINT ( 'NONE',  ( 1.653273178848927064E-15, 3.999999997815050889, -27.00000000000000355 ) ) ;
#5660 = CARTESIAN_POINT ( 'NONE',  ( -16.30427144417478402, 99.49999999999998579, 16.48895498912494517 ) ) ;
#5661 = CARTESIAN_POINT ( 'NONE',  ( 9.877377282685029372E-16, -4.781249998770965348, 2.500000000000000000 ) ) ;
#5662 = AXIS2_PLACEMENT_3D ( 'NONE', #999, #9160, #5020 ) ;
#5663 = CARTESIAN_POINT ( 'NONE',  ( 2.256430356250000546, -3.103124999385482585, 1.302750673588579877 ) ) ;
#5664 = FACE_OUTER_BOUND ( 'NONE', #9163, .T. ) ;
#5665 = EDGE_LOOP ( 'NONE', ( #9298, #7365, #8162, #4184 ) ) ;
#5666 = CARTESIAN_POINT ( 'NONE',  ( -2.256430356250000102, -4.228124999385483029, -1.302750673588580321 ) ) ;
#5667 = CARTESIAN_POINT ( 'NONE',  ( -5.039362679103552881E-15, 1.749999998907525223, 27.43301270000000258 ) ) ;
#5668 = APPLICATION_PROTOCOL_DEFINITION ( 'draft international standard', 'automotive_design', 1998, #3521 ) ;
#5669 = CYLINDRICAL_SURFACE ( 'NONE', #82, 24.00000000000000355 ) ;
#5670 = CARTESIAN_POINT ( 'NONE',  ( 1.653273178848927064E-15, 4.200000000000000178, -27.00000000000000355 ) ) ;
#5671 = VECTOR ( 'NONE', #5040, 1000.000000000000000 ) ;
#5672 = CARTESIAN_POINT ( 'NONE',  ( -20.97746206809550884, 100.0000000000000000, -11.22189255051946688 ) ) ;
#5673 = ORIENTED_EDGE ( 'NONE', *, *, #80, .T. ) ;
#5674 = CARTESIAN_POINT ( 'NONE',  ( -16.40919047799676989, 99.99999999999995737, 16.38364531277195013 ) ) ;
#5675 = CARTESIAN_POINT ( 'NONE',  ( 11.18376618407357093, 2.349999997815050090, -27.00000000000000355 ) ) ;
#5676 = CARTESIAN_POINT ( 'NONE',  ( 2.500000000000000444, -5.156249998770965348, 1.443375672974063439 ) ) ;
#5677 = CARTESIAN_POINT ( 'NONE',  ( 27.43301269999999548, 1.799999998907525045, 11.36312591709337916 ) ) ;
#5678 = CARTESIAN_POINT ( 'NONE',  ( 3.238942592553923472, 99.50000000000001421, -24.36085717291697250 ) ) ;
#5679 = APPLICATION_CONTEXT ( 'automotive_design' ) ;
#5680 = CARTESIAN_POINT ( 'NONE',  ( -11.18376618407358336, 1.149999997815050357, 26.99999999999999645 ) ) ;
#5681 = CARTESIAN_POINT ( 'NONE',  ( -2.256430356250000102, -3.440624999385482496, -1.302750673588580321 ) ) ;
#5682 = CARTESIAN_POINT ( 'NONE',  ( 8.132491713109025966, 100.0000000000000000, 21.08089001807756091 ) ) ;
#5683 = CARTESIAN_POINT ( 'NONE',  ( -16.74216497804568604, 100.0000000000000142, 15.31795814478965312 ) ) ;
#5684 = CARTESIAN_POINT ( 'NONE',  ( -7.500000000000000000, 104.5000000000000142, -3.000000000000000000 ) ) ;
#5685 = VERTEX_POINT ( 'NONE', #315 ) ;
#5686 = CARTESIAN_POINT ( 'NONE',  ( -1.249999999999998224, -4.818749998770964993, 2.165063509461097713 ) ) ;
#5687 = ORIENTED_EDGE ( 'NONE', *, *, #2754, .T. ) ;
#5688 = EDGE_CURVE ( 'NONE', #1976, #2411, #4262, .T. ) ;
#5689 = CARTESIAN_POINT ( 'NONE',  ( 4.259295290443009918, 100.0000000000000426, -24.34414156132068996 ) ) ;
#5690 = CARTESIAN_POINT ( 'NONE',  ( -1.250000000000000222, -3.224999999999999645, -2.165063509461096825 ) ) ;
#5691 = LINE ( 'NONE', #925, #10238 ) ;
#5692 = CARTESIAN_POINT ( 'NONE',  ( -1.128215178125000273, -3.365624999385482763, -1.954126010382871259 ) ) ;
#5693 = PRODUCT ( 'piston', 'piston', '', ( #2196 ) ) ;
#5694 = ORIENTED_EDGE ( 'NONE', *, *, #4115, .F. ) ;
#5695 = ORIENTED_EDGE ( 'NONE', *, *, #8350, .F. ) ;
#5696 = CARTESIAN_POINT ( 'NONE',  ( -15.18657300206754179, 99.50000000000000000, 16.26161032743331347 ) ) ;
#5697 = CARTESIAN_POINT ( 'NONE',  ( -8.673617379884035472E-16, -15.00000000000000000, 3.464101615137756163 ) ) ;
#5698 = DIRECTION ( 'NONE',  ( 0.000000000000000000, 0.9961946980917455452, -0.08715574274765836016 ) ) ;
#5699 = CARTESIAN_POINT ( 'NONE',  ( 11.36312591709336139, 5.299999998907526155, -27.43301270000000258 ) ) ;
#5700 = ORIENTED_EDGE ( 'NONE', *, *, #7539, .T. ) ;
#5701 = FACE_OUTER_BOUND ( 'NONE', #1638, .T. ) ;
#5702 = CARTESIAN_POINT ( 'NONE',  ( -21.12798922145720582, 100.0000000000000142, -10.90888695829967325 ) ) ;
#5703 = CARTESIAN_POINT ( 'NONE',  ( 1.128215178125001161, -3.253124999385482496, 1.954126010382870815 ) ) ;
#5704 = ORIENTED_EDGE ( 'NONE', *, *, #4973, .T. ) ;
#5705 = CARTESIAN_POINT ( 'NONE',  ( 4.061806280070601183, 100.0000000000000426, -22.51960061163626392 ) ) ;
#5706 = CARTESIAN_POINT ( 'NONE',  ( -4.959819536546781389E-15, 1.199999997815050401, 27.00000000000000355 ) ) ;
#5707 = ADVANCED_FACE ( 'NONE', ( #8123 ), #4241, .T. ) ;
#5708 = CARTESIAN_POINT ( 'NONE',  ( -2.341324462030736955E-15, 75.00000000000001421, 18.23673019291534558 ) ) ;
#5709 = CARTESIAN_POINT ( 'NONE',  ( 3.428794695218988053, 99.50000000000001421, -24.07607503615978572 ) ) ;
#5710 = CARTESIAN_POINT ( 'NONE',  ( 3.254133136943549776, 100.0000000000000000, -21.76036676155726823 ) ) ;
#5711 = ADVANCED_FACE ( 'NONE', ( #7474 ), #3398, .T. ) ;
#5712 = DIRECTION ( 'NONE',  ( -0.000000000000000000, 1.000000000000000000, -0.000000000000000000 ) ) ;
#5713 = CARTESIAN_POINT ( 'NONE',  ( -2.256430356249998770, -3.703124999385482674, 1.302750673588581876 ) ) ;
#5714 = CARTESIAN_POINT ( 'NONE',  ( 9.358681735871565266, 99.99999999999998579, 21.55373624431538815 ) ) ;
#5715 = ORIENTED_EDGE ( 'NONE', *, *, #9765, .F. ) ;
#5716 = CARTESIAN_POINT ( 'NONE',  ( -2.256430356249999214, -4.603124999385482141, 1.302750673588581876 ) ) ;
#5717 = PRESENTATION_STYLE_ASSIGNMENT (( #1920 ) ) ;
#5718 = CARTESIAN_POINT ( 'NONE',  ( -15.84712739808237103, 99.49999999999997158, 14.83079670662049310 ) ) ;
#5719 =( BOUNDED_SURFACE ( )  B_SPLINE_SURFACE ( 1, 2, ( 
 ( #321, #8176, #4197, #373, #3509, #6751, #9950, #8380, #1209, #4403, #9743, #5233, #1265, #9209, #2210, #4508, #3624, #5412, #7701, #10171, #3731, #481, #2039, #3057, #6804, #6857, #10053, #2890, #3008, #7021, #6238, #6075, #6129, #7759, #8433, #642, #9265, #9440, #5466, #4674, #4562, #2267, #7642, #10003, #4454, #6970, #3676, #2099, #1428, #6183, #5292, #9382, #8605, #9324, #4618, #8489, #5356, #1318, #6021, #7811, #7864, #1479, #3784, #8656, #538, #2838, #3837, #2948, #6913, #10112, #2155, #8545, #1369, #590, #10225, #5517, #7277, #3941, #3259, #7914, #6448, #748, #3994, #900, #3886, #853, #4722, #10330, #3306, #1684, #6347, #3163, #2649, #7179, #4042, #4825, #6496, #6295, #9033, #1633, #9813 ),
 ( #7126, #9542, #2366, #9637, #8709, #9493, #5839, #9586, #1850, #2418, #5563, #4091, #7073, #5615, #8754, #7226, #115, #6396, #2317, #5046, #1528, #2473, #1578, #8021, #10281, #4772, #7968, #802, #5667, #8, #694, #8856, #3211, #61, #8803, #4877, #8069, #3114, #8248, #1127, #4319, #7504, #4425, #1286, #505, #343, #396, #2003, #3484, #5258, #3533, #3699, #10078, #9290, #9184, #7668, #1903, #1075, #2701, #1232, #6668, #9864, #6042, #448, #5890, #3646, #10022, #3590, #6825, #5097, #9973, #2752, #292, #7611, #2123, #6097, #8402, #6881, #9085, #7451, #2857, #7557, #2914, #6722, #8348, #6775, #2807, #4271, #8457, #8297, #4476, #9919, #9232, #5945, #2064, #9136, #1180, #1956, #5151, #4370, #5992 ) ),
 .UNSPECIFIED., .F., .F., .T. ) 
 B_SPLINE_SURFACE_WITH_KNOTS ( ( 2, 2 ),
 ( 3, 2, 2, 2, 2, 2, 2, 2, 2, 2, 2, 2, 2, 2, 2, 2, 2, 2, 2, 2, 2, 2, 2, 2, 2, 2, 2, 2, 2, 2, 2, 2, 2, 2, 2, 2, 2, 2, 2, 2, 2, 2, 2, 2, 2, 2, 2, 2, 2, 2, 3 ),
 ( 0.000000000000000000, 1.000000000000000000 ),
 ( 0.000000000000000000, 0.01785714285714285615, 0.03571428571428571230, 0.05357142857142856845, 0.07142857142857142461, 0.08928571428571428770, 0.1071428571428571369, 0.1250000000000000000, 0.1428571428571428492, 0.1607142857142857262, 0.1785714285714285754, 0.1964285714285714246, 0.2142857142857142738, 0.2321428571428571508, 0.2500000000000000000, 0.2678571428571428492, 0.2857142857142856984, 0.3035714285714285476, 0.3214285714285714524, 0.3392857142857143016, 0.3571428571428571508, 0.3750000000000000000, 0.3928571428571428492, 0.4107142857142856984, 0.4285714285714285476, 0.4464285714285714524, 0.4642857142857143016, 0.4821428571428571508, 0.5000000000000000000, 0.5178571428571429047, 0.5357142857142856984, 0.5535714285714286031, 0.5714285714285713969, 0.5892857142857143016, 0.6071428571428570953, 0.6250000000000000000, 0.6428571428571429047, 0.6607142857142856984, 0.6785714285714286031, 0.6964285714285713969, 0.7142857142857143016, 0.7321428571428570953, 0.7500000000000000000, 0.7678571428571429047, 0.7857142857142856984, 0.8035714285714286031, 0.8214285714285713969, 0.8392857142857143016, 0.8571428571428570953, 0.8750000000000000000, 0.8928571428571429047 ),
 .UNSPECIFIED. ) 
 GEOMETRIC_REPRESENTATION_ITEM ( )  RATIONAL_B_SPLINE_SURFACE ( (
 ( 1.000000000000000000, 0.9238795325112867385, 1.000000000000000000, 0.9238795325112867385, 1.000000000000000000, 0.9238795325112867385, 1.000000000000000000, 0.9238795325112867385, 1.000000000000000000, 0.9238795325112867385, 1.000000000000000000, 0.9238795325112867385, 1.000000000000000000, 0.9238795325112867385, 1.000000000000000000, 0.9238795325112867385, 1.000000000000000000, 0.9238795325112867385, 1.000000000000000000, 0.9238795325112867385, 1.000000000000000000, 0.9238795325112867385, 1.000000000000000000, 0.9238795325112867385, 1.000000000000000000, 0.9238795325112867385, 1.000000000000000000, 0.9238795325112867385, 1.000000000000000000, 0.9238795325112867385, 1.000000000000000000, 0.9238795325112867385, 1.000000000000000000, 0.9238795325112867385, 1.000000000000000000, 0.9238795325112867385, 1.000000000000000000, 0.9238795325112867385, 1.000000000000000000, 0.9238795325112867385, 1.000000000000000000, 0.9238795325112867385, 1.000000000000000000, 0.9238795325112867385, 1.000000000000000000, 0.9238795325112867385, 1.000000000000000000, 0.9238795325112867385, 1.000000000000000000, 0.9238795325112867385, 1.000000000000000000, 0.9238795325112867385, 1.000000000000000000, 0.9238795325112867385, 1.000000000000000000, 0.9238795325112867385, 1.000000000000000000, 0.9238795325112867385, 1.000000000000000000, 0.9238795325112867385, 1.000000000000000000, 0.9238795325112867385, 1.000000000000000000, 0.9238795325112867385, 1.000000000000000000, 0.9238795325112867385, 1.000000000000000000, 0.9238795325112867385, 1.000000000000000000, 0.9238795325112867385, 1.000000000000000000, 0.9238795325112867385, 1.000000000000000000, 0.9238795325112867385, 1.000000000000000000, 0.9238795325112867385, 1.000000000000000000, 0.9238795325112867385, 1.000000000000000000, 0.9238795325112867385, 1.000000000000000000, 0.9238795325112867385, 1.000000000000000000, 0.9238795325112867385, 1.000000000000000000, 0.9238795325112867385, 1.000000000000000000, 0.9238795325112867385, 1.000000000000000000, 0.9238795325112867385, 1.000000000000000000, 0.9238795325112867385, 1.000000000000000000, 0.9238795325112867385, 1.000000000000000000, 0.9238795325112867385, 1.000000000000000000, 0.9238795325112867385, 1.000000000000000000, 0.9238795325112867385, 1.000000000000000000),
 ( 1.000000000000000000, 0.9238795325112867385, 1.000000000000000000, 0.9238795325112867385, 1.000000000000000000, 0.9238795325112867385, 1.000000000000000000, 0.9238795325112867385, 1.000000000000000000, 0.9238795325112867385, 1.000000000000000000, 0.9238795325112867385, 1.000000000000000000, 0.9238795325112867385, 1.000000000000000000, 0.9238795325112867385, 1.000000000000000000, 0.9238795325112867385, 1.000000000000000000, 0.9238795325112867385, 1.000000000000000000, 0.9238795325112867385, 1.000000000000000000, 0.9238795325112867385, 1.000000000000000000, 0.9238795325112867385, 1.000000000000000000, 0.9238795325112867385, 1.000000000000000000, 0.9238795325112867385, 1.000000000000000000, 0.9238795325112867385, 1.000000000000000000, 0.9238795325112867385, 1.000000000000000000, 0.9238795325112867385, 1.000000000000000000, 0.9238795325112867385, 1.000000000000000000, 0.9238795325112867385, 1.000000000000000000, 0.9238795325112867385, 1.000000000000000000, 0.9238795325112867385, 1.000000000000000000, 0.9238795325112867385, 1.000000000000000000, 0.9238795325112867385, 1.000000000000000000, 0.9238795325112867385, 1.000000000000000000, 0.9238795325112867385, 1.000000000000000000, 0.9238795325112867385, 1.000000000000000000, 0.9238795325112867385, 1.000000000000000000, 0.9238795325112867385, 1.000000000000000000, 0.9238795325112867385, 1.000000000000000000, 0.9238795325112867385, 1.000000000000000000, 0.9238795325112867385, 1.000000000000000000, 0.9238795325112867385, 1.000000000000000000, 0.9238795325112867385, 1.000000000000000000, 0.9238795325112867385, 1.000000000000000000, 0.9238795325112867385, 1.000000000000000000, 0.9238795325112867385, 1.000000000000000000, 0.9238795325112867385, 1.000000000000000000, 0.9238795325112867385, 1.000000000000000000, 0.9238795325112867385, 1.000000000000000000, 0.9238795325112867385, 1.000000000000000000, 0.9238795325112867385, 1.000000000000000000, 0.9238795325112867385, 1.000000000000000000, 0.9238795325112867385, 1.000000000000000000, 0.9238795325112867385, 1.000000000000000000, 0.9238795325112867385, 1.000000000000000000, 0.9238795325112867385, 1.000000000000000000, 0.9238795325112867385, 1.000000000000000000, 0.9238795325112867385, 1.000000000000000000, 0.9238795325112867385, 1.000000000000000000) ) ) 
 REPRESENTATION_ITEM ( '' )  SURFACE ( )  );
#5720 = CARTESIAN_POINT ( 'NONE',  ( -4.959819536546781389E-15, 3.000000000000000000, 27.00000000000000355 ) ) ;
#5721 = CARTESIAN_POINT ( 'NONE',  ( 2.964854786877021642, 99.50000000000000000, -22.43901021186594846 ) ) ;
#5722 = VERTEX_POINT ( 'NONE', #166 ) ;
#5723 = CARTESIAN_POINT ( 'NONE',  ( 2.500000000000000000, -3.374999999999999556, -3.061616997868383141E-16 ) ) ;
#5724 = CARTESIAN_POINT ( 'NONE',  ( -20.93486371557392545, 99.99999999999995737, -10.61231311368802466 ) ) ;
#5725 = ORIENTED_EDGE ( 'NONE', *, *, #7478, .T. ) ;
#5726 = VERTEX_POINT ( 'NONE', #3558 ) ;
#5727 = CARTESIAN_POINT ( 'NONE',  ( 2.940631318607589417, 100.0000000000000000, -23.77584808773673331 ) ) ;
#5728 = CARTESIAN_POINT ( 'NONE',  ( 0.6698729810778025762, -4.311153809338631682, 2.500000000000002665 ) ) ;
#5729 = VECTOR ( 'NONE', #8266, 1000.000000000000000 ) ;
#5730 = CARTESIAN_POINT ( 'NONE',  ( 0.000000000000000000, 0.000000000000000000, 0.000000000000000000 ) ) ;
#5731 = CARTESIAN_POINT ( 'NONE',  ( 4.786228327491940187E-16, -3.290624999385482585, 2.605501347177161087 ) ) ;
#5732 = CARTESIAN_POINT ( 'NONE',  ( 11.18376618407357093, 1.750000000000000000, -27.00000000000000355 ) ) ;
#5733 = CARTESIAN_POINT ( 'NONE',  ( 11.18376618407357093, 5.549999997815051600, -27.00000000000000355 ) ) ;
#5734 = CARTESIAN_POINT ( 'NONE',  ( 2.500000000000000000, -5.118749998770964815, -3.061616997868383141E-16 ) ) ;
#5735 = ORIENTED_EDGE ( 'NONE', *, *, #858, .T. ) ;
#5736 = CARTESIAN_POINT ( 'NONE',  ( -21.98271324694694329, 100.0000000000000000, -11.39207625356720222 ) ) ;
#5737 = DIRECTION ( 'NONE',  ( 0.8660254037844384856, 0.000000000000000000, 0.5000000000000003331 ) ) ;
#5738 = CARTESIAN_POINT ( 'NONE',  ( -22.16320288552370243, 99.50000000000001421, -10.86869938533413915 ) ) ;
#5739 = CARTESIAN_POINT ( 'NONE',  ( -2.256430356249999214, -4.153124999385482852, 1.302750673588581876 ) ) ;
#5740 = B_SPLINE_CURVE_WITH_KNOTS ( 'NONE', 1,
 ( #806, #5571 ),
 .UNSPECIFIED., .F., .F.,
 ( 2, 2 ),
 ( 0.000000000000000000, 1.000000000000000000 ),
 .UNSPECIFIED. ) ;
#5741 = ADVANCED_FACE ( 'NONE', ( #5067 ), #9942, .F. ) ;
#5742 = ORIENTED_EDGE ( 'NONE', *, *, #6076, .F. ) ;
#5743 = CARTESIAN_POINT ( 'NONE',  ( 1.250000000000001110, -1.649999999999999689, 2.165063509461096380 ) ) ;
#5744 = CARTESIAN_POINT ( 'NONE',  ( -20.42657152723830905, 99.50000000000000000, -10.54129411626120216 ) ) ;
#5745 = CARTESIAN_POINT ( 'NONE',  ( -21.79668695291220715, 100.0000000000000000, -11.08213026643738353 ) ) ;
#5746 =( GEOMETRIC_REPRESENTATION_CONTEXT ( 3 ) GLOBAL_UNCERTAINTY_ASSIGNED_CONTEXT ( ( #49 ) ) GLOBAL_UNIT_ASSIGNED_CONTEXT ( ( #5358, #7644, #6805 ) ) REPRESENTATION_CONTEXT ( 'NONE', 'WORKASPACE' ) );
#5747 = ORIENTED_EDGE ( 'NONE', *, *, #5317, .F. ) ;
#5748 = CARTESIAN_POINT ( 'NONE',  ( 3.845216150098881513, 99.50000000000000000, -21.40922359334548020 ) ) ;
#5749 = CARTESIAN_POINT ( 'NONE',  ( 3.973150561375555334, 99.50000000000000000, -22.87236500961342855 ) ) ;
#5750 = DIRECTION ( 'NONE',  ( -0.000000000000000000, -1.000000000000000000, -0.000000000000000000 ) ) ;
#5751 = ADVANCED_FACE ( 'NONE', ( #366 ), #6546, .T. ) ;
#5752 = CARTESIAN_POINT ( 'NONE',  ( 3.873456569393397331, 100.0000000000000568, -22.53291374702356364 ) ) ;
#5753 = CARTESIAN_POINT ( 'NONE',  ( 19.09188309203678102, 4.499999997815050001, 19.09188309203678813 ) ) ;
#5754 = CARTESIAN_POINT ( 'NONE',  ( -20.45905772418405988, 99.50000000000000000, -10.59533404166311321 ) ) ;
#5755 = CARTESIAN_POINT ( 'NONE',  ( -21.18972881998075763, 99.49999999999998579, -9.781869222470191971 ) ) ;
#5756 = CARTESIAN_POINT ( 'NONE',  ( -15.07178375341841381, 99.50000000000000000, 16.66969090848992607 ) ) ;
#5757 = CARTESIAN_POINT ( 'NONE',  ( -21.79668695291220715, 99.50000000000000000, -11.08213026643738353 ) ) ;
#5758 = EDGE_CURVE ( 'NONE', #2494, #4882, #8922, .T. ) ;
#5759 = CARTESIAN_POINT ( 'NONE',  ( 2.940631318607589417, 99.50000000000000000, -23.77584808773673331 ) ) ;
#5760 = ORIENTED_EDGE ( 'NONE', *, *, #4556, .F. ) ;
#5761 = CARTESIAN_POINT ( 'NONE',  ( 2.256430356249999658, -4.828124999385483562, -1.302750673588581432 ) ) ;
#5762 = EDGE_CURVE ( 'NONE', #5524, #2954, #9981, .T. ) ;
#5763 = CARTESIAN_POINT ( 'NONE',  ( -15.07178375341841381, 99.50000000000000000, 15.16157792772069790 ) ) ;
#5764 = CARTESIAN_POINT ( 'NONE',  ( -2.256430356250000102, -0.7031249993854828961, 0.000000000000000000 ) ) ;
#5765 = EDGE_CURVE ( 'NONE', #8029, #5243, #1328, .T. ) ;
#5766 = CARTESIAN_POINT ( 'NONE',  ( -27.00000000000001421, 3.650000000000000799, 11.18376618407356382 ) ) ;
#5767 = DIRECTION ( 'NONE',  ( 0.000000000000000000, 0.000000000000000000, 1.000000000000000000 ) ) ;
#5768 = DIRECTION ( 'NONE',  ( 0.000000000000000000, 1.000000000000000000, 0.000000000000000000 ) ) ;
#5769 = CARTESIAN_POINT ( 'NONE',  ( -20.91430522584054330, 99.99999999999998579, -10.19152558580213608 ) ) ;
#5770 = ORIENTED_EDGE ( 'NONE', *, *, #2927, .F. ) ;
#5771 = ORIENTED_EDGE ( 'NONE', *, *, #8962, .F. ) ;
#5772 = CARTESIAN_POINT ( 'NONE',  ( -27.43301270000000969, 4.699999998907524734, 11.36312591709335784 ) ) ;
#5773 = CARTESIAN_POINT ( 'NONE',  ( -15.91768310440539658, 99.50000000000002842, 15.18344740530786652 ) ) ;
#5774 = CARTESIAN_POINT ( 'NONE',  ( -2.256430356249998770, -2.915624999385482585, 1.302750673588581876 ) ) ;
#5775 = CARTESIAN_POINT ( 'NONE',  ( -16.49816537377288128, 100.0000000000000000, 16.70951083495554101 ) ) ;
#5776 = CIRCLE ( 'NONE', #929, 0.4999999999999953371 ) ;
#5777 = CARTESIAN_POINT ( 'NONE',  ( -1.250000000000000222, -1.875000000000000000, -2.165063509461096825 ) ) ;
#5778 = CARTESIAN_POINT ( 'NONE',  ( -1.915118561403101882, -5.394273269507308122, -1.606960141313192425 ) ) ;
#5779 = EDGE_LOOP ( 'NONE', ( #3538, #3471, #5588, #4642 ) ) ;
#5780 = CARTESIAN_POINT ( 'NONE',  ( -22.33529725360453000, 99.49999999999997158, -10.20112572733487255 ) ) ;
#5781 = CARTESIAN_POINT ( 'NONE',  ( 3.198738776810544415, 99.50000000000001421, -22.02447230026614022 ) ) ;
#5782 = CARTESIAN_POINT ( 'NONE',  ( -17.94007301623892658, 100.0000000000000000, 17.49000340848992607 ) ) ;
#5783 = CARTESIAN_POINT ( 'NONE',  ( -15.27171031718473770, 100.0000000000000284, 15.44886715306589764 ) ) ;
#5784 = CARTESIAN_POINT ( 'NONE',  ( 1.249999999999999334, -1.499999999999999778, -2.165063509461096825 ) ) ;
#5785 = VECTOR ( 'NONE', #9803, 1000.000000000000114 ) ;
#5786 = CARTESIAN_POINT ( 'NONE',  ( -4.959819536546781389E-15, 3.599999997815050534, 27.00000000000000355 ) ) ;
#5787 = EDGE_CURVE ( 'NONE', #6736, #6706, #3952, .T. ) ;
#5788 = CARTESIAN_POINT ( 'NONE',  ( -21.44539290152690114, 100.0000000000000000, -11.08070480119962298 ) ) ;
#5789 = ORIENTED_EDGE ( 'NONE', *, *, #8577, .T. ) ;
#5790 = ADVANCED_FACE ( 'NONE', ( #579 ), #6065, .T. ) ;
#5791 = CARTESIAN_POINT ( 'NONE',  ( 0.000000000000000000, 100.0000000000000000, 0.000000000000000000 ) ) ;
#5792 = VECTOR ( 'NONE', #2393, 999.9999999999998863 ) ;
#5793 = MECHANICAL_DESIGN_GEOMETRIC_PRESENTATION_REPRESENTATION (  '', ( #7982 ), #798 ) ;
#5794 = CARTESIAN_POINT ( 'NONE',  ( 3.024867170474271116, 99.49999999999995737, -24.05477125543085748 ) ) ;
#5795 = CARTESIAN_POINT ( 'NONE',  ( 7.812290123947159159, 99.49999999999998579, 21.17203503082402349 ) ) ;
#5796 = ORIENTED_EDGE ( 'NONE', *, *, #5633, .T. ) ;
#5797 = DIRECTION ( 'NONE',  ( -8.881784197001252323E-16, 0.000000000000000000, -1.000000000000000000 ) ) ;
#5798 = CARTESIAN_POINT ( 'NONE',  ( -11.18376618407358336, 4.349999997815050534, 26.99999999999999645 ) ) ;
#5799 = DIRECTION ( 'NONE',  ( -0.000000000000000000, 1.000000000000000000, -0.000000000000000000 ) ) ;
#5800 = CARTESIAN_POINT ( 'NONE',  ( -21.13452028402337035, 99.50000000000000000, -9.824917503107416294 ) ) ;
#5801 = DIRECTION ( 'NONE',  ( -0.000000000000000000, -1.000000000000000000, -0.000000000000000000 ) ) ;
#5802 = CARTESIAN_POINT ( 'NONE',  ( -21.93524539549613550, 99.49999999999998579, -11.03420246938663318 ) ) ;
#5803 = CARTESIAN_POINT ( 'NONE',  ( 2.864934851235464208, 100.0000000000000000, -21.80148171563692827 ) ) ;
#5804 = CARTESIAN_POINT ( 'NONE',  ( 0.000000000000000000, 100.0000000000000000, 0.000000000000000000 ) ) ;
#5805 = EDGE_CURVE ( 'NONE', #9070, #3821, #5313, .T. ) ;
#5806 = ORIENTED_EDGE ( 'NONE', *, *, #8836, .F. ) ;
#5807 = CARTESIAN_POINT ( 'NONE',  ( 1.128215178124999607, -4.340624999385482852, -1.954126010382871259 ) ) ;
#5808 = FILL_AREA_STYLE_COLOUR ( '', #4139 ) ;
#5809 = CARTESIAN_POINT ( 'NONE',  ( -1.249999999999998224, -2.624999999999999556, 2.165063509461097713 ) ) ;
#5810 = CARTESIAN_POINT ( 'NONE',  ( 2.958578797724396026, 99.50000000000000000, -23.36432507653281121 ) ) ;
#5811 = CARTESIAN_POINT ( 'NONE',  ( 27.43301270000000258, 3.449999998907525178, 0.000000000000000000 ) ) ;
#5812 = CARTESIAN_POINT ( 'NONE',  ( -27.00000000000000355, 0.3499999999999999778, -11.18376618407357270 ) ) ;
#5813 = DIRECTION ( 'NONE',  ( 0.000000000000000000, 0.000000000000000000, -1.000000000000000000 ) ) ;
#5814 = AXIS2_PLACEMENT_3D ( 'NONE', #10086, #9297, #8409 ) ;
#5815 = CARTESIAN_POINT ( 'NONE',  ( 0.000000000000000000, 100.0000000000000000, 0.000000000000000000 ) ) ;
#5816 = CARTESIAN_POINT ( 'NONE',  ( -20.91264567078791714, 99.49999999999997158, -10.54226115003387676 ) ) ;
#5817 = ORIENTED_EDGE ( 'NONE', *, *, #7794, .F. ) ;
#5818 = CARTESIAN_POINT ( 'NONE',  ( -20.95972469638759250, 99.99999999999994316, -9.536167108072199028 ) ) ;
#5819 = CARTESIAN_POINT ( 'NONE',  ( 1.679787559701184688E-15, 5.249999998907525445, -27.43301270000000258 ) ) ;
#5820 = CARTESIAN_POINT ( 'NONE',  ( -15.37731512048643268, 99.50000000000000000, 15.34394520743122214 ) ) ;
#5821 = VECTOR ( 'NONE', #10133, 1000.000000000000000 ) ;
#5822 = CARTESIAN_POINT ( 'NONE',  ( 3.949943451936506644, 100.0000000000000000, -21.41482314084395711 ) ) ;
#5823 = CARTESIAN_POINT ( 'NONE',  ( 9.482997300390421103, 99.50000000000000000, 20.28643943712827991 ) ) ;
#5824 = DIRECTION ( 'NONE',  ( 0.000000000000000000, -1.000000000000000000, 0.000000000000000000 ) ) ;
#5825 = FACE_OUTER_BOUND ( 'NONE', #9786, .T. ) ;
#5826 = EDGE_LOOP ( 'NONE', ( #7838, #977, #6271, #1512 ) ) ;
#5827 = CARTESIAN_POINT ( 'NONE',  ( 5.302876193624534821E-16, -5.231249998770965526, 2.886751345948128655 ) ) ;
#5828 = ORIENTED_EDGE ( 'NONE', *, *, #69, .F. ) ;
#5829 = EDGE_CURVE ( 'NONE', #6080, #3756, #1754, .T. ) ;
#5830 = CARTESIAN_POINT ( 'NONE',  ( 3.771794781161601939, 99.99999999999998579, -21.07813736596861176 ) ) ;
#5831 = CARTESIAN_POINT ( 'NONE',  ( 3.356341388373609291, 99.99999999999998579, -21.61643044175963979 ) ) ;
#5832 = CARTESIAN_POINT ( 'NONE',  ( 3.891852272358404807, 99.50000000000001421, -22.89765557720719968 ) ) ;
#5833 = CARTESIAN_POINT ( 'NONE',  ( -15.15623813234777018, 100.0000000000000000, 16.19783826294960249 ) ) ;
#5834 = CARTESIAN_POINT ( 'NONE',  ( 8.067960508813904141, 99.50000000000000000, 20.80952186068213905 ) ) ;
#5835 = CARTESIAN_POINT ( 'NONE',  ( -7.500000000000000000, 104.5000000000000142, -0.9999999999999997780 ) ) ;
#5836 = CARTESIAN_POINT ( 'NONE',  ( -21.65488089977124275, 99.99999999999997158, -11.10326233039539723 ) ) ;
#5837 = ORIENTED_EDGE ( 'NONE', *, *, #6677, .T. ) ;
#5838 = LINE ( 'NONE', #5045, #10077 ) ;
#5839 = CARTESIAN_POINT ( 'NONE',  ( -19.39806930854667755, 0.6499999989075252449, -19.39806930854668110 ) ) ;
#5840 = CARTESIAN_POINT ( 'NONE',  ( 4.996790860652426159E-15, -2.306249998770965259, -2.500000000000000000 ) ) ;
#5841 = CARTESIAN_POINT ( 'NONE',  ( 4.122675185292913547, 99.49999999999997158, -22.83451320417363561 ) ) ;
#5842 = CARTESIAN_POINT ( 'NONE',  ( 3.775125937424839151, 99.99999999999997158, -21.41825520325024712 ) ) ;
#5843 = CARTESIAN_POINT ( 'NONE',  ( 2.859712287474666770, 99.50000000000000000, -22.17872625191749236 ) ) ;
#5844 = CARTESIAN_POINT ( 'NONE',  ( -19.09188309203678813, 5.099999997815051422, 19.09188309203678457 ) ) ;
#5845 = CARTESIAN_POINT ( 'NONE',  ( 1.045839947578414805E-15, -0.5625000000000001110, -2.500000000000000000 ) ) ;
#5846 = CARTESIAN_POINT ( 'NONE',  ( -21.52330660073277002, 100.0000000000000142, -9.647028226243550719 ) ) ;
#5847 = CARTESIAN_POINT ( 'NONE',  ( 4.061354557346970040, 99.99999999999997158, -22.84864678426182039 ) ) ;
#5848 = CARTESIAN_POINT ( 'NONE',  ( -21.79668695291220715, 100.0000000000000000, -11.08213026643738353 ) ) ;
#5849 = PLANE ( 'NONE',  #1627 ) ;
#5850 = CARTESIAN_POINT ( 'NONE',  ( -1.250000000000000222, -0.07499999999999999722, -2.165063509461096825 ) ) ;
#5851 = VERTEX_POINT ( 'NONE', #3249 ) ;
#5852 = MECHANICAL_DESIGN_GEOMETRIC_PRESENTATION_REPRESENTATION (  '', ( #4352 ), #7037 ) ;
#5853 = CARTESIAN_POINT ( 'NONE',  ( -2.256430356250000102, -4.190624999385482496, 0.000000000000000000 ) ) ;
#5854 = SURFACE_STYLE_FILL_AREA ( #2525 ) ;
#5855 = DIRECTION ( 'NONE',  ( 0.000000000000000000, -1.000000000000000000, 0.000000000000000000 ) ) ;
#5856 = CARTESIAN_POINT ( 'NONE',  ( 2.936358689207804851, 100.0000000000000000, -23.74786164940363875 ) ) ;
#5857 = CARTESIAN_POINT ( 'NONE',  ( -11.36312591709335962, 3.699999998907525622, -27.43301270000000258 ) ) ;
#5858 = ADVANCED_FACE ( 'NONE', ( #3104 ), #8701, .T. ) ;
#5859 = LINE ( 'NONE', #1874, #6100 ) ;
#5860 =( REPRESENTATION_RELATIONSHIP ('NONE','NONE', #3375, #5114 ) REPRESENTATION_RELATIONSHIP_WITH_TRANSFORMATION ( #1514 )SHAPE_REPRESENTATION_RELATIONSHIP( ) );
#5861 = CARTESIAN_POINT ( 'NONE',  ( 4.640952353770416927, 100.0000000000000000, -24.17064508475253604 ) ) ;
#5862 = FILL_AREA_STYLE ('',( #2669 ) ) ;
#5863 = ORIENTED_EDGE ( 'NONE', *, *, #8659, .T. ) ;
#5864 = CARTESIAN_POINT ( 'NONE',  ( -21.89277277937676303, 99.99999999999992895, -9.329958722595300458 ) ) ;
#5865 = CARTESIAN_POINT ( 'NONE',  ( 9.676361905416719367, 99.50000000000000000, 21.63547735782115211 ) ) ;
#5866 = CARTESIAN_POINT ( 'NONE',  ( 9.358681735871565266, 99.49999999999998579, 21.55373624431538815 ) ) ;
#5867 = CARTESIAN_POINT ( 'NONE',  ( -2.499999999999999112, -1.706249998770965615, 1.443375672974065882 ) ) ;
#5868 = CARTESIAN_POINT ( 'NONE',  ( -16.35834224700816009, 100.0000000000000142, 16.43761959438736397 ) ) ;
#5869 = CARTESIAN_POINT ( 'NONE',  ( 3.403200340195960738, 99.49999999999998579, -22.39827506699316118 ) ) ;
#5870 = ADVANCED_BREP_SHAPE_REPRESENTATION ( '', ( #2806, #5055 ), #7312 ) ;
#5871 = CARTESIAN_POINT ( 'NONE',  ( 0.000000000000000000, 100.0000000000000000, 0.000000000000000000 ) ) ;
#5872 = ORIENTED_EDGE ( 'NONE', *, *, #6253, .F. ) ;
#5873 = CARTESIAN_POINT ( 'NONE',  ( 0.000000000000000000, 100.0000000000000000, -27.00000000000000355 ) ) ;
#5874 = AXIS2_PLACEMENT_3D ( 'NONE', #1502, #2975, #6370 ) ;
#5875 = CARTESIAN_POINT ( 'NONE',  ( 1.250000000000001110, -3.843749998770965348, 2.165063509461096380 ) ) ;
#5876 = VERTEX_POINT ( 'NONE', #9485 ) ;
#5877 = CARTESIAN_POINT ( 'NONE',  ( -22.33391032228853490, 100.0000000000000000, -10.55243757774135993 ) ) ;
#5878 = CARTESIAN_POINT ( 'NONE',  ( 3.399971579580567393, 99.99999999999997158, -21.57509867787664248 ) ) ;
#5879 = DIRECTION ( 'NONE',  ( -0.000000000000000000, 1.000000000000000000, -0.000000000000000000 ) ) ;
#5880 = CARTESIAN_POINT ( 'NONE',  ( -15.19031985176477662, 99.99999999999998579, 15.56880617076518547 ) ) ;
#5881 = EDGE_CURVE ( 'NONE', #5950, #3778, #3420, .T. ) ;
#5882 = AXIS2_PLACEMENT_3D ( 'NONE', #4737, #6509, #8769 ) ;
#5883 = EDGE_CURVE ( 'NONE', #3601, #519, #3931, .T. ) ;
#5884 = ORIENTED_EDGE ( 'NONE', *, *, #9664, .T. ) ;
#5885 = CARTESIAN_POINT ( 'NONE',  ( 8.122452352567329115, 99.50000000000000000, 21.04970292111833530 ) ) ;
#5886 = LINE ( 'NONE', #8291, #7482 ) ;
#5887 = DIRECTION ( 'NONE',  ( 0.000000000000000000, -1.000000000000000000, 0.000000000000000000 ) ) ;
#5888 = CARTESIAN_POINT ( 'NONE',  ( 2.500000000000000444, -2.512500000000000178, 1.443375672974063439 ) ) ;
#5889 = VERTEX_POINT ( 'NONE', #10318 ) ;
#5890 = CARTESIAN_POINT ( 'NONE',  ( 27.43301270000000258, 3.549999998907525267, 0.000000000000000000 ) ) ;
#5891 = LINE ( 'NONE', #7505, #2223 ) ;
#5892 = CARTESIAN_POINT ( 'NONE',  ( 3.750007936853901658, 99.50000000000001421, -22.95001988029826734 ) ) ;
#5893 = CARTESIAN_POINT ( 'NONE',  ( 8.051038018032482313, 99.49999999999998579, 19.92675698219059299 ) ) ;
#5894 = VERTEX_POINT ( 'NONE', #5657 ) ;
#5895 = DIRECTION ( 'NONE',  ( -0.8547548816071318667, 0.000000000000000000, 0.5190318799156541374 ) ) ;
#5896 = CARTESIAN_POINT ( 'NONE',  ( 27.00000000000000355, 4.599999997815050534, 0.000000000000000000 ) ) ;
#5897 = CARTESIAN_POINT ( 'NONE',  ( -20.61566945723384592, 99.50000000000000000, -10.83949095114527594 ) ) ;
#5898 = CARTESIAN_POINT ( 'NONE',  ( -21.08523985030068459, 100.0000000000000000, -9.874866134143449159 ) ) ;
#5899 = CARTESIAN_POINT ( 'NONE',  ( 3.328702480760086235, 99.99999999999997158, -23.35145716610488975 ) ) ;
#5900 = CARTESIAN_POINT ( 'NONE',  ( -21.30928386698190025, 99.50000000000000000, -11.02857376369709996 ) ) ;
#5901 = CARTESIAN_POINT ( 'NONE',  ( 4.909381318607588973, 100.0000000000000000, -23.54377677363417121 ) ) ;
#5902 = CARTESIAN_POINT ( 'NONE',  ( -1.728530063377412107, -5.141148402510967053, -1.450400555903694988 ) ) ;
#5903 = CARTESIAN_POINT ( 'NONE',  ( 2.500000000000000000, -0.6749999999999999334, -3.061616997868383141E-16 ) ) ;
#5904 = CARTESIAN_POINT ( 'NONE',  ( -14.83363727892122519, 100.0000000000000000, 15.50654517199034466 ) ) ;
#5905 = DIRECTION ( 'NONE',  ( 0.000000000000000000, -1.000000000000000000, 0.000000000000000000 ) ) ;
#5906 = CARTESIAN_POINT ( 'NONE',  ( -11.36312591709337383, 1.599999998907525534, 27.43301269999999548 ) ) ;
#5907 = CARTESIAN_POINT ( 'NONE',  ( -3.486133158594716510E-16, -1.012499999999999956, -2.500000000000000000 ) ) ;
#5908 = DIRECTION ( 'NONE',  ( 0.000000000000000000, -1.000000000000000000, 0.000000000000000000 ) ) ;
#5909 = CARTESIAN_POINT ( 'NONE',  ( 21.82251602564102910, 99.50000000000000000, -0.5181290064102563875 ) ) ;
#5910 = CARTESIAN_POINT ( 'NONE',  ( -11.18376618407356737, 4.049999997815050712, -27.00000000000000355 ) ) ;
#5911 = EDGE_LOOP ( 'NONE', ( #10260, #57, #1439, #6444 ) ) ;
#5912 =( BOUNDED_CURVE ( )  B_SPLINE_CURVE ( 2, ( #10134, #5318, #3695, #10018, #10195, #2853, #10073, #1337, #2802 ),
 .UNSPECIFIED., .F., .T. ) 
 B_SPLINE_CURVE_WITH_KNOTS ( ( 3, 2, 2, 2, 3 ),
 ( 0.3958333333333333703, 0.4027777777777777901, 0.4166666666666666852, 0.4305555555555555802, 0.4375000000000000000 ),
 .UNSPECIFIED. ) 
 CURVE ( )  GEOMETRIC_REPRESENTATION_ITEM ( )  RATIONAL_B_SPLINE_CURVE ( ( 0.9330127018922194093, 0.9330127018922196314, 1.000000000000000000, 0.8660254037844387076, 1.000000000000000000, 0.8660254037844387076, 1.000000000000000000, 0.9330127018922194093, 0.9330127018922194093 ) ) 
 REPRESENTATION_ITEM ( '' )  );
#5913 = CARTESIAN_POINT ( 'NONE',  ( 7.729958523985794194, 99.50000000000001421, 20.63140804260154937 ) ) ;
#5914 = CARTESIAN_POINT ( 'NONE',  ( 0.000000000000000000, -15.00000000000000000, -2.500000000000000000 ) ) ;
#5915 = FACE_OUTER_BOUND ( 'NONE', #1339, .T. ) ;
#5916 = EDGE_CURVE ( 'NONE', #9964, #3939, #1571, .T. ) ;
#5917 = CARTESIAN_POINT ( 'NONE',  ( -21.43094455402013310, 100.0000000000000000, -11.42705968398779426 ) ) ;
#5918 = CARTESIAN_POINT ( 'NONE',  ( 4.446585460023182890, 100.0000000000000284, -21.79057454014859019 ) ) ;
#5919 = CARTESIAN_POINT ( 'NONE',  ( -22.59920249870969045, 99.99999999999998579, -10.80326527670058567 ) ) ;
#5920 = CARTESIAN_POINT ( 'NONE',  ( -20.97771390646102319, 100.0000000000000284, -10.03345247102482674 ) ) ;
#5921 = ORIENTED_EDGE ( 'NONE', *, *, #9652, .F. ) ;
#5922 = CARTESIAN_POINT ( 'NONE',  ( 4.887668416326221177, 100.0000000000000142, -23.70513093767710089 ) ) ;
#5923 = CARTESIAN_POINT ( 'NONE',  ( 1.128215178125001161, -2.353124999385482585, 1.954126010382870815 ) ) ;
#5924 = ORIENTED_EDGE ( 'NONE', *, *, #3496, .F. ) ;
#5925 = CARTESIAN_POINT ( 'NONE',  ( -22.28244091826395135, 99.50000000000000000, -10.68852969318427881 ) ) ;
#5926 = CARTESIAN_POINT ( 'NONE',  ( 3.231466532446834350, 99.49999999999997158, -21.81145066552309686 ) ) ;
#5927 = AXIS2_PLACEMENT_3D ( 'NONE', #8406, #3862, #4482 ) ;
#5928 = ADVANCED_FACE ( 'NONE', ( #9533 ), #4590, .T. ) ;
#5929 = CARTESIAN_POINT ( 'NONE',  ( 3.269123371500344710, 99.50000000000001421, -23.64665713169964434 ) ) ;
#5930 = CARTESIAN_POINT ( 'NONE',  ( 4.295198626299897349, 99.50000000000000000, -24.68029520312135006 ) ) ;
#5931 = ORIENTED_EDGE ( 'NONE', *, *, #2318, .T. ) ;
#5932 = B_SPLINE_CURVE_WITH_KNOTS ( 'NONE', 3,
 ( #301, #5003, #3490, #6533, #1033, #4179, #9721, #5897, #1858, #5754, #2655 ),
 .UNSPECIFIED., .F., .F.,
 ( 4, 1, 1, 1, 1, 1, 1, 1, 4 ),
 ( 0.000000000000000000, 0.09767211715481777246, 0.1989896052561311024, 0.3043518128873296535, 0.4150874769980872347, 0.5363819683935961979, 0.6738601886791220075, 0.8283091006677448798, 1.000000000000000000 ),
 .UNSPECIFIED. ) ;
#5933 = ADVANCED_FACE ( 'NONE', ( #3342 ), #2596, .F. ) ;
#5934 = ORIENTED_EDGE ( 'NONE', *, *, #5432, .F. ) ;
#5935 = AXIS2_PLACEMENT_3D ( 'NONE', #4278, #3385, #2562 ) ;
#5936 = CARTESIAN_POINT ( 'NONE',  ( -16.49092618789450526, 99.99999999999995737, 16.26472549871478179 ) ) ;
#5937 = CARTESIAN_POINT ( 'NONE',  ( 2.500000000000000000, -0.6187499987709659255, -3.061616997868383141E-16 ) ) ;
#5938 = ADVANCED_FACE ( 'NONE', ( #8111 ), #6675, .T. ) ;
#5939 = CARTESIAN_POINT ( 'NONE',  ( -21.51485068221570174, 100.0000000000000000, -11.09552232883975087 ) ) ;
#5940 = AXIS2_PLACEMENT_3D ( 'NONE', #6258, #3180, #9458 ) ;
#5941 = CARTESIAN_POINT ( 'NONE',  ( 9.834295043520187463, 100.0000000000000284, 21.14079655679390513 ) ) ;
#5942 = ORIENTED_EDGE ( 'NONE', *, *, #5305, .T. ) ;
#5943 = EDGE_CURVE ( 'NONE', #6493, #8517, #9040, .T. ) ;
#5944 = DIRECTION ( 'NONE',  ( 0.000000000000000000, 0.000000000000000000, 1.000000000000000000 ) ) ;
#5945 = CARTESIAN_POINT ( 'NONE',  ( 11.36312591709336850, 4.999999998907526333, 27.43301269999999903 ) ) ;
#5946 = CARTESIAN_POINT ( 'NONE',  ( 5.825495487346713297, 99.50000000000000000, 20.69456627699299744 ) ) ;
#5947 = CARTESIAN_POINT ( 'NONE',  ( 3.293272160652527258, 99.49999999999997158, -24.41359064397622802 ) ) ;
#5948 = CARTESIAN_POINT ( 'NONE',  ( 8.223467485077383898, 99.49999999999997158, 19.78581333328655134 ) ) ;
#5949 = ADVANCED_FACE ( 'NONE', ( #8203 ), #8158, .T. ) ;
#5950 = VERTEX_POINT ( 'NONE', #349 ) ;
#5951 = CARTESIAN_POINT ( 'NONE',  ( 9.910564025336874749, 99.50000000000001421, 20.75459158945058036 ) ) ;
#5952 = CARTESIAN_POINT ( 'NONE',  ( -19.09188309203678457, 2.499999997815050445, -19.09188309203678813 ) ) ;
#5953 = CARTESIAN_POINT ( 'NONE',  ( -21.31369174262763622, 99.49999999999997158, -9.710155485040722567 ) ) ;
#5954 = FACE_OUTER_BOUND ( 'NONE', #7501, .T. ) ;
#5955 = VERTEX_POINT ( 'NONE', #5104 ) ;
#5956 = CARTESIAN_POINT ( 'NONE',  ( 4.901590909071964042, 100.0000000000000000, -23.62641080846013608 ) ) ;
#5957 = CARTESIAN_POINT ( 'NONE',  ( -1.250000000000000222, -4.968749998770965348, -2.165063509461096825 ) ) ;
#5958 = ORIENTED_EDGE ( 'NONE', *, *, #172, .T. ) ;
#5959 = EDGE_CURVE ( 'NONE', #2588, #9964, #5932, .T. ) ;
#5960 = AXIS2_PLACEMENT_3D ( 'NONE', #6197, #8444, #10185 ) ;
#5961 = CARTESIAN_POINT ( 'NONE',  ( 5.302876193624534821E-16, -0.7874999999999998668, 2.886751345948128655 ) ) ;
#5962 = FACE_OUTER_BOUND ( 'NONE', #1040, .T. ) ;
#5963 = CARTESIAN_POINT ( 'NONE',  ( -27.43301270000000258, 1.449999998907525178, -3.359575119402369376E-15 ) ) ;
#5964 = LINE ( 'NONE', #8421, #1852 ) ;
#5965 = AXIS2_PLACEMENT_3D ( 'NONE', #3108, #4872, #742 ) ;
#5966 = CARTESIAN_POINT ( 'NONE',  ( 9.877377282685029372E-16, -1.237499999999999600, 2.500000000000000000 ) ) ;
#5967 = LINE ( 'NONE', #4242, #4820 ) ;
#5968 = CARTESIAN_POINT ( 'NONE',  ( 1.653273178848927064E-15, 1.000000000000000000, -27.00000000000000355 ) ) ;
#5969 = CARTESIAN_POINT ( 'NONE',  ( 7.734522023158566739, 99.50000000000002842, 20.86022014488863618 ) ) ;
#5970 = CARTESIAN_POINT ( 'NONE',  ( -22.10910773081910818, 99.50000000000001421, -11.33820747227609793 ) ) ;
#5971 = CARTESIAN_POINT ( 'NONE',  ( -1.128215178125000273, -0.6656249993854829183, -1.954126010382871259 ) ) ;
#5972 = CARTESIAN_POINT ( 'NONE',  ( -2.256430356250000102, -0.1406249993854829794, 0.000000000000000000 ) ) ;
#5973 = APPLICATION_PROTOCOL_DEFINITION ( 'draft international standard', 'automotive_design', 1998, #4070 ) ;
#5974 = CARTESIAN_POINT ( 'NONE',  ( -16.60513711880303234, 99.50000000000001421, 15.15667007515659748 ) ) ;
#5975 = DIRECTION ( 'NONE',  ( 0.000000000000000000, -1.000000000000000000, 0.000000000000000000 ) ) ;
#5976 = CARTESIAN_POINT ( 'NONE',  ( -21.80427673524616239, 100.0000000000000000, -9.663674634844889866 ) ) ;
#5977 = ADVANCED_FACE ( 'NONE', ( #8303 ), #5054, .T. ) ;
#5978 = PLANE ( 'NONE',  #4213 ) ;
#5979 = CARTESIAN_POINT ( 'NONE',  ( 4.786228327491941173E-16, -1.490624999385482985, 2.605501347177161087 ) ) ;
#5980 = EDGE_LOOP ( 'NONE', ( #6218, #10233, #6919, #10256 ) ) ;
#5981 = CARTESIAN_POINT ( 'NONE',  ( -22.25406130147340633, 99.50000000000002842, -9.998337329044998611 ) ) ;
#5982 = CARTESIAN_POINT ( 'NONE',  ( -5.039362679103552881E-15, 0.8499999989075253115, 27.43301270000000258 ) ) ;
#5983 = CARTESIAN_POINT ( 'NONE',  ( 21.47055288461538325, 100.0000000000000000, -0.7081330128205128860 ) ) ;
#5984 = CARTESIAN_POINT ( 'NONE',  ( -19.09188309203678813, 3.499999997815050445, 19.09188309203678457 ) ) ;
#5985 = EDGE_CURVE ( 'NONE', #10235, #4027, #4228, .T. ) ;
#5986 = CARTESIAN_POINT ( 'NONE',  ( 4.835062408351179286, 99.50000000000000000, -21.79588013901878440 ) ) ;
#5987 = DIRECTION ( 'NONE',  ( -0.000000000000000000, 1.000000000000000000, -0.000000000000000000 ) ) ;
#5988 = CARTESIAN_POINT ( 'NONE',  ( 2.500000000000000000, -2.474999999999999645, -3.061616997868383141E-16 ) ) ;
#5989 = VERTEX_POINT ( 'NONE', #8942 ) ;
#5990 = B_SPLINE_CURVE_WITH_KNOTS ( 'NONE', 3,
 ( #6047, #5441, #9412, #5265, #6887, #9236, #8576, #4483, #8633, #10028, #2864, #7730, #6215, #8407, #2187, #2128, #1291, #9295, #7674 ),
 .UNSPECIFIED., .F., .F.,
 ( 4, 1, 1, 1, 1, 1, 1, 1, 1, 1, 1, 1, 1, 1, 1, 1, 4 ),
 ( 0.000000000000000000, 0.06533929434940796699, 0.1284421010879715219, 0.1894557237235162950, 0.2487158350925330053, 0.3070727012892665031, 0.3650088636856013702, 0.4229902474982629723, 0.4815891416229265420, 0.5404453987529589387, 0.6002338948610608238, 0.6608164219703346332, 0.7232441343194829786, 0.7881366429682739039, 0.8556965829275263724, 0.9259544997225339635, 1.000000000000000000 ),
 .UNSPECIFIED. ) ;
#5991 = CARTESIAN_POINT ( 'NONE',  ( -3.486133158594716510E-16, -2.756249998770965437, -2.500000000000000000 ) ) ;
#5992 = CARTESIAN_POINT ( 'NONE',  ( 1.679787559701184688E-15, 5.349999998907525089, -27.43301270000000258 ) ) ;
#5993 = LINE ( 'NONE', #449, #6558 ) ;
#5994 =( REPRESENTATION_RELATIONSHIP ('NONE','NONE', #3375, #9736 ) REPRESENTATION_RELATIONSHIP_WITH_TRANSFORMATION ( #6334 )SHAPE_REPRESENTATION_RELATIONSHIP( ) );
#5995 = CARTESIAN_POINT ( 'NONE',  ( 9.802580223201115217, 99.49999999999997158, 21.25247094773282086 ) ) ;
#5996 = ORIENTED_EDGE ( 'NONE', *, *, #5048, .F. ) ;
#5997 = CARTESIAN_POINT ( 'NONE',  ( -20.77412980915959650, 99.99999999999997158, -9.759484723497815040 ) ) ;
#5998 = DIRECTION ( 'NONE',  ( 0.000000000000000000, -1.000000000000000000, 0.000000000000000000 ) ) ;
#5999 = FACE_BOUND ( 'NONE', #7018, .T. ) ;
#6000 = CARTESIAN_POINT ( 'NONE',  ( 4.154273145530666511, 100.0000000000000000, -22.82723029927519676 ) ) ;
#6001 = ORIENTED_EDGE ( 'NONE', *, *, #9143, .T. ) ;
#6002 = CARTESIAN_POINT ( 'NONE',  ( -16.35834224700816009, 100.0000000000000142, 16.43761959438736397 ) ) ;
#6003 = CARTESIAN_POINT ( 'NONE',  ( -27.43301270000000969, 2.399999998907525356, 11.36312591709335784 ) ) ;
#6004 = ORIENTED_EDGE ( 'NONE', *, *, #322, .T. ) ;
#6005 = CARTESIAN_POINT ( 'NONE',  ( 2.500000000000000444, -2.062499999999999556, 1.443375672974063439 ) ) ;
#6006 = CARTESIAN_POINT ( 'NONE',  ( 3.311778287470797721, 99.50000000000000000, -21.22295334266859967 ) ) ;
#6007 = CARTESIAN_POINT ( 'NONE',  ( -1.128215178124998497, -2.428124999385482763, 1.954126010382872147 ) ) ;
#6008 = ADVANCED_FACE ( 'NONE', ( #986 ), #9769, .T. ) ;
#6009 = CARTESIAN_POINT ( 'NONE',  ( 1.679787559701184688E-15, 3.649999998907525356, -27.43301270000000258 ) ) ;
#6010 = DIRECTION ( 'NONE',  ( 0.000000000000000000, 0.000000000000000000, 1.000000000000000000 ) ) ;
#6011 = ORIENTED_EDGE ( 'NONE', *, *, #3329, .F. ) ;
#6012 = EDGE_CURVE ( 'NONE', #3495, #570, #3541, .T. ) ;
#6013 = CARTESIAN_POINT ( 'NONE',  ( 8.961048541867139505, 100.0000000000000142, 19.57961630251783092 ) ) ;
#6014 = CARTESIAN_POINT ( 'NONE',  ( -4.357666448243394824E-15, -2.981249998770965526, 2.500000000000000000 ) ) ;
#6015 = CARTESIAN_POINT ( 'NONE',  ( 8.051038018032482313, 99.99999999999998579, 19.92675698219059299 ) ) ;
#6016 = CARTESIAN_POINT ( 'NONE',  ( -15.43596444985078975, 100.0000000000000284, 15.30036492734783593 ) ) ;
#6017 = CARTESIAN_POINT ( 'NONE',  ( -2.256430356249998770, -1.003124999385482718, 1.302750673588581876 ) ) ;
#6018 = CARTESIAN_POINT ( 'NONE',  ( 2.852289972453743161, 100.0000000000000000, -22.14293542748032451 ) ) ;
#6019 = ORIENTED_EDGE ( 'NONE', *, *, #4805, .F. ) ;
#6020 = CARTESIAN_POINT ( 'NONE',  ( 2.256430356250000546, -0.8531249993854828073, 1.302750673588579877 ) ) ;
#6021 = CARTESIAN_POINT ( 'NONE',  ( -19.39806930854668465, 3.149999998907525356, 19.39806930854667755 ) ) ;
#6022 =( LENGTH_UNIT ( ) NAMED_UNIT ( * ) SI_UNIT ( .MILLI., .METRE. ) );
#6023 = ORIENTED_EDGE ( 'NONE', *, *, #5530, .T. ) ;
#6024 = CARTESIAN_POINT ( 'NONE',  ( 4.232447118646125439, 99.99999999999998579, -21.54138831197867887 ) ) ;
#6025 = CARTESIAN_POINT ( 'NONE',  ( 3.282077632710153292, 99.50000000000000000, -23.74569985055724786 ) ) ;
#6026 = FACE_OUTER_BOUND ( 'NONE', #3290, .T. ) ;
#6027 = ORIENTED_EDGE ( 'NONE', *, *, #843, .F. ) ;
#6028 = DIRECTION ( 'NONE',  ( -0.04357787137382922171, -0.9961946980917455452, 0.07547908730517349785 ) ) ;
#6029 = CARTESIAN_POINT ( 'NONE',  ( 2.256430356250000546, -2.765624999385483118, 1.302750673588579877 ) ) ;
#6030 = ORIENTED_EDGE ( 'NONE', *, *, #4456, .F. ) ;
#6031 = CARTESIAN_POINT ( 'NONE',  ( -21.96365545856212265, 99.50000000000001421, -9.726658277667754149 ) ) ;
#6032 = CARTESIAN_POINT ( 'NONE',  ( -15.07178375341841559, 99.50000000000001421, 15.16157792772069968 ) ) ;
#6033 = CARTESIAN_POINT ( 'NONE',  ( 5.243816414761435674, 99.50000000000000000, -23.48558366465980995 ) ) ;
#6034 =( BOUNDED_CURVE ( )  B_SPLINE_CURVE ( 2, ( #8268, #1924, #1096, #5812, #9003, #1975, #9103, #314, #5171 ),
 .UNSPECIFIED., .F., .T. ) 
 B_SPLINE_CURVE_WITH_KNOTS ( ( 3, 2, 2, 2, 3 ),
 ( 0.03571428571428571230, 0.05357142857142856845, 0.07142857142857142461, 0.08928571428571428770, 0.1071428571428571369 ),
 .UNSPECIFIED. ) 
 CURVE ( )  GEOMETRIC_REPRESENTATION_ITEM ( )  RATIONAL_B_SPLINE_CURVE ( ( 1.000000000000000000, 0.9238795325112867385, 1.000000000000000000, 0.9238795325112867385, 1.000000000000000000, 0.9238795325112867385, 1.000000000000000000, 0.9238795325112867385, 1.000000000000000000 ) ) 
 REPRESENTATION_ITEM ( '' )  );
#6035 = VERTEX_POINT ( 'NONE', #5845 ) ;
#6036 = AXIS2_PLACEMENT_3D ( 'NONE', #4288, #1047, #6639 ) ;
#6037 = CARTESIAN_POINT ( 'NONE',  ( -2.500000000000000000, -0.8812499987709659921, -1.443375672974064106 ) ) ;
#6038 = CARTESIAN_POINT ( 'NONE',  ( -16.65546786808457469, 99.99999999999998579, 16.57295196178722918 ) ) ;
#6039 = CARTESIAN_POINT ( 'NONE',  ( 0.6698729810778075722, -3.017403810567666156, 2.499999999999999556 ) ) ;
#6040 = VERTEX_POINT ( 'NONE', #5708 ) ;
#6041 = CARTESIAN_POINT ( 'NONE',  ( 11.18376618407357626, 1.249999997815050445, 27.00000000000000000 ) ) ;
#6042 = CARTESIAN_POINT ( 'NONE',  ( 19.39806930854667399, 3.449999998907525622, 19.39806930854668465 ) ) ;
#6043 = AXIS2_PLACEMENT_3D ( 'NONE', #2808, #1904, #7558 ) ;
#6044 = EDGE_CURVE ( 'NONE', #8336, #4987, #7407, .T. ) ;
#6045 = CARTESIAN_POINT ( 'NONE',  ( 9.838488147574068421, 99.50000000000000000, 20.25735696016189280 ) ) ;
#6046 = CARTESIAN_POINT ( 'NONE',  ( 7.486453019397995234, 99.50000000000000000, 23.81666162955709964 ) ) ;
#6047 = CARTESIAN_POINT ( 'NONE',  ( 4.295198626299898237, 99.50000000000001421, -24.68029520312135361 ) ) ;
#6048 = CARTESIAN_POINT ( 'NONE',  ( -1.249999999999998224, -3.918749998770965082, 2.165063509461097713 ) ) ;
#6049 = CARTESIAN_POINT ( 'NONE',  ( -16.37951318544778445, 99.49999999999997158, 15.41600550949200077 ) ) ;
#6050 = CARTESIAN_POINT ( 'NONE',  ( -0.6698729810778063509, -0.5424038105676658450, -2.500000000000000000 ) ) ;
#6051 = ORIENTED_EDGE ( 'NONE', *, *, #9851, .F. ) ;
#6052 = DIRECTION ( 'NONE',  ( 0.000000000000000000, -0.000000000000000000, 1.000000000000000000 ) ) ;
#6053 = CARTESIAN_POINT ( 'NONE',  ( -19.39806930854668465, 1.649999998907525356, 19.39806930854667755 ) ) ;
#6054 = ORIENTED_EDGE ( 'NONE', *, *, #4045, .F. ) ;
#6055 = CARTESIAN_POINT ( 'NONE',  ( 2.500000000000000000, -2.024999999999999911, -3.061616997868383141E-16 ) ) ;
#6056 = EDGE_CURVE ( 'NONE', #4212, #6063, #3063, .T. ) ;
#6057 = CARTESIAN_POINT ( 'NONE',  ( 9.357295078982289738, 99.50000000000004263, 20.12145687760884627 ) ) ;
#6058 = CARTESIAN_POINT ( 'NONE',  ( 3.023131990384279710, 99.50000000000002842, -21.47496011329876708 ) ) ;
#6059 = CARTESIAN_POINT ( 'NONE',  ( 1.128215178124999607, -2.203124999385482674, -1.954126010382871259 ) ) ;
#6060 = CARTESIAN_POINT ( 'NONE',  ( -11.36312591709335962, 4.499999998907525445, -27.43301270000000258 ) ) ;
#6061 = CARTESIAN_POINT ( 'NONE',  ( -19.39806930854667755, 2.249999998907525001, -19.39806930854668110 ) ) ;
#6062 = COLOUR_RGB ( '',0.8941176470588234615, 0.8941176470588234615, 0.8941176470588234615 ) ;
#6064 = ORIENTED_EDGE ( 'NONE', *, *, #5142, .F. ) ;
#6063 = VERTEX_POINT ( 'NONE', #6162 ) ;
#6065 = PLANE ( 'NONE',  #5620 ) ;
#6066 = CARTESIAN_POINT ( 'NONE',  ( 1.034219503716432668E-14, -3.206249998770966059, -2.500000000000000000 ) ) ;
#6067 = CARTESIAN_POINT ( 'NONE',  ( 7.812290123947159159, 99.99999999999998579, 21.17203503082402349 ) ) ;
#6068 = CARTESIAN_POINT ( 'NONE',  ( 3.664124300404482337, 100.0000000000000284, -24.27219056640880623 ) ) ;
#6069 = VERTEX_POINT ( 'NONE', #3598 ) ;
#6070 = CARTESIAN_POINT ( 'NONE',  ( -2.256430356249998770, -0.5531249993854828739, 1.302750673588581876 ) ) ;
#6071 = CARTESIAN_POINT ( 'NONE',  ( -9.703070624755296135E-15, -5.231249998770965526, 2.500000000000000444 ) ) ;
#6072 = EDGE_CURVE ( 'NONE', #369, #6174, #2010, .T. ) ;
#6073 = CARTESIAN_POINT ( 'NONE',  ( -2.500000000000000000, -1.293749998770965970, 0.000000000000000000 ) ) ;
#6074 = PRESENTATION_LAYER_ASSIGNMENT (  '', '', ( #9429 ) ) ;
#6075 = CARTESIAN_POINT ( 'NONE',  ( 27.43301269999999548, 1.799999998907525267, 11.36312591709337738 ) ) ;
#6076 = EDGE_CURVE ( 'NONE', #6802, #2896, #1187, .T. ) ;
#6077 = CARTESIAN_POINT ( 'NONE',  ( -15.98658610793439117, 99.99999999999997158, 14.83943845084690949 ) ) ;
#6078 = CARTESIAN_POINT ( 'NONE',  ( 27.00000000000000355, 0.8000000000000000444, 0.000000000000000000 ) ) ;
#6079 = CARTESIAN_POINT ( 'NONE',  ( 2.859712287474666770, 99.50000000000000000, -22.17872625191749236 ) ) ;
#6080 = VERTEX_POINT ( 'NONE', #8578 ) ;
#6081 = EDGE_LOOP ( 'NONE', ( #9325, #9322, #2994, #8019 ) ) ;
#6082 = EDGE_CURVE ( 'NONE', #6810, #4141, #10085, .T. ) ;
#6083 = CARTESIAN_POINT ( 'NONE',  ( -16.05266356869597644, 99.50000000000000000, 16.62382211633880047 ) ) ;
#6084 = CARTESIAN_POINT ( 'NONE',  ( -2.256430356250000102, -2.503124999385482496, 0.000000000000000000 ) ) ;
#6085 = ORIENTED_EDGE ( 'NONE', *, *, #6915, .F. ) ;
#6086 = CARTESIAN_POINT ( 'NONE',  ( -22.28738277804067636, 99.99999999999994316, -10.06255608345902886 ) ) ;
#6087 = CARTESIAN_POINT ( 'NONE',  ( 2.500000000000000444, -0.7124999999999999112, 1.443375672974063439 ) ) ;
#6088 = CARTESIAN_POINT ( 'NONE',  ( 1.249999999999999334, -0.1499999999999999944, -2.165063509461096825 ) ) ;
#6089 = CARTESIAN_POINT ( 'NONE',  ( 2.256430356250000102, -2.278124999385482852, -2.763330213280484622E-16 ) ) ;
#6090 = CARTESIAN_POINT ( 'NONE',  ( 3.375079225685456041, 100.0000000000000000, -22.79123997459842954 ) ) ;
#6091 = VECTOR ( 'NONE', #989, 1000.000000000000227 ) ;
#6092 = VERTEX_POINT ( 'NONE', #9360 ) ;
#6093 = CARTESIAN_POINT ( 'NONE',  ( 4.280752963211088336, 99.49999999999997158, -21.16602454745684270 ) ) ;
#6094 = CYLINDRICAL_SURFACE ( 'NONE', #4951, 23.99999999999999645 ) ;
#6095 = CARTESIAN_POINT ( 'NONE',  ( 24.91446314102564230, 99.50000000000000000, -1.581029647435897578 ) ) ;
#6096 = DIRECTION ( 'NONE',  ( 0.000000000000000000, -1.000000000000000000, 0.000000000000000000 ) ) ;
#6097 = CARTESIAN_POINT ( 'NONE',  ( -11.36312591709337383, 4.099999998907525089, 27.43301269999999548 ) ) ;
#6098 = CARTESIAN_POINT ( 'NONE',  ( -2.256430356250000102, -1.490624999385482763, 0.000000000000000000 ) ) ;
#6099 = FACE_OUTER_BOUND ( 'NONE', #5382, .T. ) ;
#6100 = VECTOR ( 'NONE', #214, 1000.000000000000000 ) ;
#6101 = ORIENTED_EDGE ( 'NONE', *, *, #3337, .F. ) ;
#6102 = CARTESIAN_POINT ( 'NONE',  ( -21.49703851962343037, 99.99999999999997158, -9.300281078773625865 ) ) ;
#6103 = CARTESIAN_POINT ( 'NONE',  ( 0.000000000000000000, 97.50000000000000000, 0.000000000000000000 ) ) ;
#6104 = CARTESIAN_POINT ( 'NONE',  ( -2.499999999999999112, -3.956249998770965615, 1.443375672974065882 ) ) ;
#6105 = LINE ( 'NONE', #2244, #1483 ) ;
#6106 = EDGE_CURVE ( 'NONE', #1163, #1380, #6928, .T. ) ;
#6107 = ORIENTED_EDGE ( 'NONE', *, *, #2496, .T. ) ;
#6108 = CARTESIAN_POINT ( 'NONE',  ( -15.84348323231452049, 100.0000000000000000, 15.18005498687102772 ) ) ;
#6109 = CARTESIAN_POINT ( 'NONE',  ( -27.43301270000000258, 1.499999998907525223, -11.36312591709336317 ) ) ;
#6110 = ORIENTED_EDGE ( 'NONE', *, *, #7485, .T. ) ;
#6111 = CARTESIAN_POINT ( 'NONE',  ( -1.249999999999998224, -2.624999999999999556, 2.165063509461097713 ) ) ;
#6112 = CARTESIAN_POINT ( 'NONE',  ( 0.000000000000000000, 0.000000000000000000, 0.000000000000000000 ) ) ;
#6113 = CARTESIAN_POINT ( 'NONE',  ( 8.973011566395204142, 99.49999999999997158, 19.93291184930431115 ) ) ;
#6114 = DIRECTION ( 'NONE',  ( 0.000000000000000000, 0.000000000000000000, -1.000000000000000000 ) ) ;
#6115 = CARTESIAN_POINT ( 'NONE',  ( -1.128215178124998497, -2.878124999385482496, 1.954126010382872147 ) ) ;
#6116 = CARTESIAN_POINT ( 'NONE',  ( 4.773458297025112707, 99.50000000000001421, -24.02094923175124208 ) ) ;
#6117 = CARTESIAN_POINT ( 'NONE',  ( 19.39806930854668110, 2.849999998907525089, -19.39806930854668110 ) ) ;
#6118 = ORIENTED_EDGE ( 'NONE', *, *, #7406, .F. ) ;
#6119 = CARTESIAN_POINT ( 'NONE',  ( 9.725694684612619767, 100.0000000000000000, 20.03234812723199454 ) ) ;
#6120 = CARTESIAN_POINT ( 'NONE',  ( 3.023131990384279710, 99.50000000000002842, -21.47496011329876708 ) ) ;
#6121 = ADVANCED_FACE ( 'NONE', ( #9144 ), #2188, .F. ) ;
#6122 = CARTESIAN_POINT ( 'NONE',  ( -16.36254897777739004, 100.0000000000000142, 15.39785597259249350 ) ) ;
#6123 = VECTOR ( 'NONE', #4465, 1000.000000000000114 ) ;
#6124 = ORIENTED_EDGE ( 'NONE', *, *, #2448, .T. ) ;
#6125 = CARTESIAN_POINT ( 'NONE',  ( 2.256430356249999658, -2.128124999385482496, -1.302750673588581432 ) ) ;
#6126 = CARTESIAN_POINT ( 'NONE',  ( -21.84904385032055174, 99.49999999999998579, -11.42736543092427404 ) ) ;
#6127 = ORIENTED_EDGE ( 'NONE', *, *, #5166, .T. ) ;
#6128 = CARTESIAN_POINT ( 'NONE',  ( 9.877377282685029372E-16, -1.631249998770965659, 2.500000000000000000 ) ) ;
#6129 = CARTESIAN_POINT ( 'NONE',  ( 27.43301270000000258, 1.849999998907525312, 0.000000000000000000 ) ) ;
#6130 = B_SPLINE_CURVE_WITH_KNOTS ( 'NONE', 3,
 ( #7774, #6090, #8448, #1278, #8619, #4579, #5310 ),
 .UNSPECIFIED., .F., .F.,
 ( 4, 1, 1, 1, 4 ),
 ( 0.000000000000000000, 0.2581490702850675056, 0.5078756004687992043, 0.7540928115589713432, 1.000000000000000000 ),
 .UNSPECIFIED. ) ;
#6131 = ORIENTED_EDGE ( 'NONE', *, *, #2179, .F. ) ;
#6132 = DIRECTION ( 'NONE',  ( -0.000000000000000000, 1.000000000000000000, -0.000000000000000000 ) ) ;
#6133 = CARTESIAN_POINT ( 'NONE',  ( -4.959819536546781389E-15, 0.6000000000000000888, 27.00000000000000355 ) ) ;
#6134 = AXIS2_PLACEMENT_3D ( 'NONE', #96, #882, #7950 ) ;
#6135 = CARTESIAN_POINT ( 'NONE',  ( 9.446088657802272692, 100.0000000000000711, 20.22669104216016578 ) ) ;
#6136 = VERTEX_POINT ( 'NONE', #9296 ) ;
#6137 = CARTESIAN_POINT ( 'NONE',  ( -16.49419651247312046, 99.99999999999994316, 15.57134447358898477 ) ) ;
#6138 = CARTESIAN_POINT ( 'NONE',  ( 8.067960508813904141, 99.50000000000000000, 20.80952186068213905 ) ) ;
#6139 = CARTESIAN_POINT ( 'NONE',  ( 2.256430356250000546, -1.415624999385482807, 1.302750673588579877 ) ) ;
#6140 = ORIENTED_EDGE ( 'NONE', *, *, #780, .F. ) ;
#6141 = CARTESIAN_POINT ( 'NONE',  ( -3.000000000000000888, -15.00000000000000000, 1.732050807568878303 ) ) ;
#6142 = CARTESIAN_POINT ( 'NONE',  ( -27.43301270000000258, 0.5999999989075253115, -11.36312591709336317 ) ) ;
#6143 = PRODUCT_DEFINITION_FORMATION_WITH_SPECIFIED_SOURCE ( 'ANY', '', #1592, .NOT_KNOWN. ) ;
#6144 = CARTESIAN_POINT ( 'NONE',  ( -22.28244091826395135, 99.50000000000000000, -10.68852969318427881 ) ) ;
#6145 = CARTESIAN_POINT ( 'NONE',  ( -1.595409442497313560E-16, -2.165624999385483029, -2.605501347177161087 ) ) ;
#6146 = CARTESIAN_POINT ( 'NONE',  ( 5.207032889226773875, 100.0000000000000284, -23.83708953234284778 ) ) ;
#6147 = LINE ( 'NONE', #2175, #6945 ) ;
#6148 = EDGE_CURVE ( 'NONE', #6813, #3209, #9377, .T. ) ;
#6149 = VECTOR ( 'NONE', #1875, 1000.000000000000000 ) ;
#6150 = LINE ( 'NONE', #7551, #8329 ) ;
#6151 = CARTESIAN_POINT ( 'NONE',  ( -16.92301558088953328, 100.0000000000000142, 15.88693424423437683 ) ) ;
#6152 = CARTESIAN_POINT ( 'NONE',  ( 1.034219503716432668E-14, -2.812500000000000444, -2.500000000000000000 ) ) ;
#6153 = ORIENTED_EDGE ( 'NONE', *, *, #2021, .F. ) ;
#6154 = CARTESIAN_POINT ( 'NONE',  ( 0.000000000000000000, 0.000000000000000000, -2.500000000000000000 ) ) ;
#6155 = CARTESIAN_POINT ( 'NONE',  ( 1.034219503716432668E-14, -4.556249998770965703, -2.500000000000000000 ) ) ;
#6156 = CARTESIAN_POINT ( 'NONE',  ( 2.256430356250000546, -2.653124999385482852, 1.302750673588579877 ) ) ;
#6157 = VECTOR ( 'NONE', #9808, 1000.000000000000000 ) ;
#6158 = CARTESIAN_POINT ( 'NONE',  ( 9.676361905416721143, 99.50000000000001421, 21.63547735782115566 ) ) ;
#6159 = EDGE_LOOP ( 'NONE', ( #4945, #4004, #10207, #10117 ) ) ;
#6160 = LINE ( 'NONE', #9358, #771 ) ;
#6161 = CARTESIAN_POINT ( 'NONE',  ( 8.857094148306096315, 100.0000000000000142, 19.57755665027156766 ) ) ;
#6162 = CARTESIAN_POINT ( 'NONE',  ( 1.653273178848927064E-15, 3.400000000000000355, -27.00000000000000355 ) ) ;
#6163 = CARTESIAN_POINT ( 'NONE',  ( -16.45635306197508996, 99.50000000000000000, 15.51056558312563105 ) ) ;
#6164 = ORIENTED_EDGE ( 'NONE', *, *, #3035, .F. ) ;
#6165 = FACE_OUTER_BOUND ( 'NONE', #8609, .T. ) ;
#6166 = CARTESIAN_POINT ( 'NONE',  ( -5.039362679103552881E-15, 2.549999998907525267, 27.43301270000000258 ) ) ;
#6167 = ORIENTED_EDGE ( 'NONE', *, *, #5557, .T. ) ;
#6168 = CARTESIAN_POINT ( 'NONE',  ( -2.500000000000000000, -3.600000000000000089, 0.000000000000000000 ) ) ;
#6169 = DIRECTION ( 'NONE',  ( 0.000000000000000000, 0.000000000000000000, 1.000000000000000000 ) ) ;
#6170 = CARTESIAN_POINT ( 'NONE',  ( 2.500000000000000000, -3.787499999999999645, -1.443375672974065438 ) ) ;
#6171 = CARTESIAN_POINT ( 'NONE',  ( -1.128215178125000273, -3.028124999385482408, -1.954126010382871259 ) ) ;
#6172 = CARTESIAN_POINT ( 'NONE',  ( -16.81182640597031508, 99.50000000000000000, 16.36129326314865295 ) ) ;
#6173 = CARTESIAN_POINT ( 'NONE',  ( 27.43301270000000258, 3.549999998907525267, 0.000000000000000000 ) ) ;
#6174 = VERTEX_POINT ( 'NONE', #7731 ) ;
#6175 = CARTESIAN_POINT ( 'NONE',  ( 8.857094148306096315, 100.0000000000000142, 19.57755665027156766 ) ) ;
#6176 = LINE ( 'NONE', #685, #7831 ) ;
#6177 = CARTESIAN_POINT ( 'NONE',  ( 3.311778287470797721, 99.50000000000000000, -21.22295334266859967 ) ) ;
#6178 = B_SPLINE_SURFACE_WITH_KNOTS ( 'NONE', 3, 1, ( 
 ( #1757, #9817 ),
 ( #9139, #5842 ),
 ( #9717, #1030 ),
 ( #4999, #2704 ),
 ( #8199, #9037 ),
 ( #1131, #1854 ),
 ( #5050, #4323 ),
 ( #937, #4954 ),
 ( #8155, #983 ),
 ( #7357, #399 ),
 ( #2388, #6365 ),
 ( #3905, #7144 ),
 ( #8725, #1388 ),
 ( #4739, #606 ),
 ( #4581, #7092 ) ),
 .UNSPECIFIED., .F., .F., .F.,
 ( 4, 1, 1, 1, 1, 1, 1, 1, 1, 1, 1, 1, 4 ),
 ( 2, 2 ),
 ( 0.000000000000000000, 0.1166921615859537187, 0.2277195327244859735, 0.3361971884410420164, 0.4453256767247914527, 0.5018483577356800396, 0.5617326728321133666, 0.6243107931132723110, 0.6909729641497043273, 0.7615676753376537933, 0.8363829297815326136, 0.9156607463298391814, 0.9999999999999998890 ),
 ( 0.000000000000000000, 1.000000000000000000 ),
 .UNSPECIFIED. ) ;
#6179 = CARTESIAN_POINT ( 'NONE',  ( -20.96643530928959365, 99.99999999999997158, -10.05541671241504886 ) ) ;
#6180 = CARTESIAN_POINT ( 'NONE',  ( -1.128215178125000273, -1.115624999385482985, -1.954126010382871259 ) ) ;
#6181 = CARTESIAN_POINT ( 'NONE',  ( 4.633286773149219329, 100.0000000000000284, -21.44575434969419447 ) ) ;
#6182 = CARTESIAN_POINT ( 'NONE',  ( 2.256430356250000546, -0.4031249993854829627, 1.302750673588579877 ) ) ;
#6183 = CARTESIAN_POINT ( 'NONE',  ( 27.43301270000000258, 2.699999998907525178, -11.36312591709336139 ) ) ;
#6184 = B_SPLINE_CURVE_WITH_KNOTS ( 'NONE', 3,
 ( #8734, #3237, #35, #3969, #3190, #6372, #3285, #4069, #4700, #7252, #2344, #6424, #3917, #9615, #5543, #723, #2399, #3087, #2449 ),
 .UNSPECIFIED., .F., .F.,
 ( 4, 1, 1, 1, 1, 1, 1, 1, 1, 1, 1, 1, 1, 1, 1, 1, 4 ),
 ( 0.000000000000000000, 0.06441145199513656494, 0.1272798026707614161, 0.1891796676955485867, 0.2501048626594916668, 0.3106574229659737063, 0.3727353219478334867, 0.4357106927796215445, 0.5001540812204312569, 0.5646670943021733224, 0.6273118991093056263, 0.6892359343283066542, 0.7500873997029591234, 0.8110709007071082999, 0.8723115105649058565, 0.9354174373376444862, 1.000000000000000000 ),
 .UNSPECIFIED. ) ;
#6185 = ORIENTED_EDGE ( 'NONE', *, *, #3430, .T. ) ;
#6186 = CARTESIAN_POINT ( 'NONE',  ( -15.70584307919286893, 99.50000000000000000, 14.84247401567675162 ) ) ;
#6187 = ADVANCED_FACE ( 'NONE', ( #5386 ), #2186, .T. ) ;
#6188 = CARTESIAN_POINT ( 'NONE',  ( -11.18376618407358336, 1.350000000000000089, 26.99999999999999645 ) ) ;
#6189 = CARTESIAN_POINT ( 'NONE',  ( 2.852289972453743161, 100.0000000000000000, -22.14293542748032451 ) ) ;
#6190 = ORIENTED_EDGE ( 'NONE', *, *, #9667, .T. ) ;
#6191 = CARTESIAN_POINT ( 'NONE',  ( 0.000000000000000000, 70.00000000000000000, 23.99999999999999645 ) ) ;
#6192 = CARTESIAN_POINT ( 'NONE',  ( -15.49014769301379069, 99.99999999999997158, 16.56834637662448273 ) ) ;
#6193 = ORIENTED_EDGE ( 'NONE', *, *, #3622, .F. ) ;
#6194 = CARTESIAN_POINT ( 'NONE',  ( 4.786228327491941173E-16, -3.290624999385482585, 2.605501347177161087 ) ) ;
#6195 = ORIENTED_EDGE ( 'NONE', *, *, #2683, .F. ) ;
#6196 = ORIENTED_EDGE ( 'NONE', *, *, #8045, .F. ) ;
#6197 = CARTESIAN_POINT ( 'NONE',  ( 0.000000000000000000, 72.50000000000001421, 0.000000000000000000 ) ) ;
#6198 = DIRECTION ( 'NONE',  ( -0.9804671828129908340, 0.000000000000000000, 0.1966827481675937905 ) ) ;
#6199 = AXIS2_PLACEMENT_3D ( 'NONE', #7616, #6944, #2762 ) ;
#6200 = CARTESIAN_POINT ( 'NONE',  ( -2.256430356250000102, -2.053124999385482763, 0.000000000000000000 ) ) ;
#6201 = CARTESIAN_POINT ( 'NONE',  ( 5.240996349771887886, 99.50000000000001421, -23.60769396873743631 ) ) ;
#6202 = CARTESIAN_POINT ( 'NONE',  ( 0.000000000000000000, 100.0000000000000000, 0.000000000000000000 ) ) ;
#6203 = APPLICATION_CONTEXT ( 'automotive_design' ) ;
#6204 = CARTESIAN_POINT ( 'NONE',  ( 5.302876193624534821E-16, -2.981249998770965970, 2.886751345948128655 ) ) ;
#6205 = ORIENTED_EDGE ( 'NONE', *, *, #1880, .T. ) ;
#6206 = CARTESIAN_POINT ( 'NONE',  ( -16.63177974700816009, 100.0000000000000000, 16.59747536361813403 ) ) ;
#6207 = CARTESIAN_POINT ( 'NONE',  ( 0.000000000000000000, -5.000000000000000000, -30.00000000000000000 ) ) ;
#6208 = ADVANCED_FACE ( 'NONE', ( #1403 ), #513, .F. ) ;
#6209 = DIRECTION ( 'NONE',  ( 0.000000000000000000, 0.000000000000000000, -1.000000000000000000 ) ) ;
#6210 = CARTESIAN_POINT ( 'NONE',  ( -1.128215178124998497, -2.315624999385482941, 1.954126010382872147 ) ) ;
#6211 = EDGE_CURVE ( 'NONE', #9263, #906, #5537, .T. ) ;
#6212 = AXIS2_PLACEMENT_3D ( 'NONE', #3965, #7151, #9564 ) ;
#6213 = ORIENTED_EDGE ( 'NONE', *, *, #8716, .F. ) ;
#6214 = CARTESIAN_POINT ( 'NONE',  ( -2.499999999999999112, -0.8062499987709659255, 1.443375672974065882 ) ) ;
#6215 = CARTESIAN_POINT ( 'NONE',  ( 5.142436925601051811, 99.49999999999995737, -24.04117066426968563 ) ) ;
#6216 = CARTESIAN_POINT ( 'NONE',  ( 3.282077632710153292, 100.0000000000000000, -23.74569985055724786 ) ) ;
#6217 = CARTESIAN_POINT ( 'NONE',  ( -16.54512803120131181, 99.50000000000000000, 16.13427955854364626 ) ) ;
#6218 = ORIENTED_EDGE ( 'NONE', *, *, #7457, .F. ) ;
#6219 = CARTESIAN_POINT ( 'NONE',  ( -15.37731512048643268, 100.0000000000000000, 15.34394520743122214 ) ) ;
#6220 = MANIFOLD_SOLID_BREP ( 'Cut-Extrude1', #6475 ) ;
#6221 = CARTESIAN_POINT ( 'NONE',  ( -27.43301270000000969, 0.7999999989075252671, 11.36312591709335784 ) ) ;
#6222 = ORIENTED_EDGE ( 'NONE', *, *, #1549, .T. ) ;
#6223 = CARTESIAN_POINT ( 'NONE',  ( -2.500000000000000000, -4.973640350848739011, -0.9099175284171376887 ) ) ;
#6224 = FACE_OUTER_BOUND ( 'NONE', #3706, .T. ) ;
#6225 = CARTESIAN_POINT ( 'NONE',  ( -2.256430356249999214, -1.115624999385482763, 1.302750673588581876 ) ) ;
#6226 = CARTESIAN_POINT ( 'NONE',  ( 1.679787559701184688E-15, 5.249999998907525445, -27.43301270000000258 ) ) ;
#6227 = CARTESIAN_POINT ( 'NONE',  ( 27.43301270000000258, 2.799999998907525267, -11.36312591709336139 ) ) ;
#6228 = ORIENTED_EDGE ( 'NONE', *, *, #184, .T. ) ;
#6229 = VECTOR ( 'NONE', #8281, 1000.000000000000000 ) ;
#6230 = CARTESIAN_POINT ( 'NONE',  ( -15.55395551812965671, 100.0000000000000284, 16.59868653893595791 ) ) ;
#6231 = PLANE ( 'NONE',  #3159 ) ;
#6232 = CARTESIAN_POINT ( 'NONE',  ( 3.356341388373609291, 99.50000000000001421, -21.61643044175963979 ) ) ;
#6233 = CARTESIAN_POINT ( 'NONE',  ( 3.286905236079108672, 100.0000000000000426, -23.77014634954566574 ) ) ;
#6234 = CARTESIAN_POINT ( 'NONE',  ( -1.595409442497313560E-16, -1.153124999385482852, -2.605501347177161087 ) ) ;
#6235 = CARTESIAN_POINT ( 'NONE',  ( -21.49703851962343037, 99.49999999999997158, -9.300281078773625865 ) ) ;
#6236 = EDGE_LOOP ( 'NONE', ( #6658, #9594, #10061, #8627, #5401 ) ) ;
#6237 = CARTESIAN_POINT ( 'NONE',  ( -1.128215178124998497, -1.415624999385482807, 1.954126010382872147 ) ) ;
#6238 = CARTESIAN_POINT ( 'NONE',  ( 19.39806930854667399, 1.749999998907525223, 19.39806930854668465 ) ) ;
#6239 = VECTOR ( 'NONE', #7362, 1000.000000000000000 ) ;
#6240 =( NAMED_UNIT ( * ) PLANE_ANGLE_UNIT ( ) SI_UNIT ( $, .RADIAN. ) );
#6241 = VERTEX_POINT ( 'NONE', #5443 ) ;
#6242 = CARTESIAN_POINT ( 'NONE',  ( 2.500000000000000444, -2.906249998770965792, 1.443375672974063439 ) ) ;
#6243 = CARTESIAN_POINT ( 'NONE',  ( -27.00000000000001421, 2.049999999999999822, 11.18376618407356382 ) ) ;
#6244 = CARTESIAN_POINT ( 'NONE',  ( 9.114876806416853938, 100.0000000000000142, 19.97295714941878231 ) ) ;
#6245 = ORIENTED_EDGE ( 'NONE', *, *, #5881, .F. ) ;
#6246 = CARTESIAN_POINT ( 'NONE',  ( -16.41302370085497131, 99.99999999999994316, 15.45185748370271206 ) ) ;
#6247 = CARTESIAN_POINT ( 'NONE',  ( 8.337740814200648387, 99.50000000000002842, 20.10843643765939248 ) ) ;
#6248 = STYLED_ITEM ( 'NONE', ( #8071 ), #4015 ) ;
#6249 = ORIENTED_EDGE ( 'NONE', *, *, #7410, .T. ) ;
#6250 = CARTESIAN_POINT ( 'NONE',  ( 1.128215178124999607, -4.003124999385482496, -1.954126010382871259 ) ) ;
#6251 = ORIENTED_EDGE ( 'NONE', *, *, #1973, .T. ) ;
#6252 = EDGE_LOOP ( 'NONE', ( #1382, #10087, #8181, #7130 ) ) ;
#6253 = EDGE_CURVE ( 'NONE', #5722, #7541, #5158, .T. ) ;
#6254 = CARTESIAN_POINT ( 'NONE',  ( 1.679787559701184688E-15, 2.049999998907525711, -27.43301270000000258 ) ) ;
#6255 = CARTESIAN_POINT ( 'NONE',  ( -21.94169572595625795, 99.50000000000000000, -9.715372641902229489 ) ) ;
#6256 = CARTESIAN_POINT ( 'NONE',  ( -2.256430356250000102, -2.090624999385482852, -1.302750673588580321 ) ) ;
#6257 = CARTESIAN_POINT ( 'NONE',  ( -19.09188309203678457, 3.500000000000000000, -19.09188309203678813 ) ) ;
#6258 = CARTESIAN_POINT ( 'NONE',  ( 0.000000000000000000, 100.0000000000000000, 0.000000000000000000 ) ) ;
#6259 = MANIFOLD_SOLID_BREP ( 'Cavity1', #10150 ) ;
#6260 = VECTOR ( 'NONE', #6764, 1000.000000000000000 ) ;
#6261 = CARTESIAN_POINT ( 'NONE',  ( 2.500000000000000444, -2.906249998770965792, 1.443375672974063439 ) ) ;
#6262 = EDGE_CURVE ( 'NONE', #2471, #8902, #10306, .T. ) ;
#6263 = CARTESIAN_POINT ( 'NONE',  ( 4.259295290443009918, 99.50000000000002842, -24.34414156132068996 ) ) ;
#6264 = CARTESIAN_POINT ( 'NONE',  ( 11.18376618407357626, 0.6500000000000001332, 27.00000000000000000 ) ) ;
#6265 =( BOUNDED_SURFACE ( )  B_SPLINE_SURFACE ( 1, 2, ( 
 ( #2038, #4507, #10170, #3623, #3007, #7700, #372, #6182, #8327, #4347, #6750, #7530, #3564, #10002, #5971, #9164, #4453, #8379, #425, #6020, #5232, #8432, #1264, #693, #7225, #10329, #1478, #7020, #4041, #7810, #7967, #10224, #9585, #7178, #6237, #7913, #5411, #5562, #4673, #3056, #3258, #4771, #8655, #9439, #4824, #8020, #6394, #747, #60, #7863, #3885, #9636, #10279, #3113, #6447, #801, #8604, #8708, #2316, #3993, #8753, #2266, #7072, #9492, #6294, #7, #852, #5464, #1427, #2417, #6346, #3210, #640, #4616, #5614, #3836, #5516, #1527, #4721, #3940, #8802, #7125, #3162, #9541, #1577, #2365, #1632, #948, #2662, #4235, #7323, #8209, #7367, #8067, #114, #4185, #3305, #8949, #9685, #1728, #5012, #7276, #2568, #208, #4142, #6495, #992, #161, #5853, #5666, #3394, #3349, #5807, #9047, #8163, #899, #4284, #2524, #1041, #5716, #6541, #4876, #5061, #7416, #8262, #5761, #9729, #1768, #4090, #1817, #8903, #6585, #4921, #256, #4963, #8117, #9776 ),
 ( #2613, #8855, #8998, #3443, #1866, #1092, #6634, #9830, #7467, #309, #3497, #6683, #2472, #1683, #9304, #3661, #5113, #6894, #5903, #6789, #1247, #5961, #6841, #2715, #8472, #410, #2768, #7625, #10036, #1143, #2136, #9153, #3605, #1969, #465, #5165, #8311, #10091, #8364, #5337, #1195, #2928, #4437, #7572, #4386, #3549, #6737, #7518, #1299, #1353, #2873, #8528, #9989, #2824, #6055, #6005, #9935, #9198, #2020, #7682, #571, #2079, #9246, #5217, #8416, #4543, #5273, #4490, #520, #4334, #6111, #3711, #7738, #9099, #3765, #9876, #1919, #359, #10155, #1409, #10311, #2988, #9423, #10208, #3097, #8587, #2351, #8741, #9476, #4755, #5549, #1464, #3977, #9366, #10162, #9572, #6168, #7112, #2405, #2195, #5395, #6280, #1513, #4707, #5599, #7057, #2304, #5501, #8004, #7163, #4601, #3196, #3043, #733, #7899, #9526, #6378, #8789, #7793, #3147, #1614, #625, #3823, #8692, #3925, #6332, #4809, #10265, #1564, #7953, #835, #6952, #7004, #6223, #2250, #785, #5448 ) ),
 .UNSPECIFIED., .F., .F., .F. ) 
 B_SPLINE_SURFACE_WITH_KNOTS ( ( 2, 2 ),
 ( 3, 2, 2, 2, 2, 2, 2, 2, 2, 2, 2, 2, 2, 2, 2, 2, 2, 2, 2, 2, 2, 2, 2, 2, 2, 2, 2, 2, 2, 2, 2, 2, 2, 2, 2, 2, 2, 2, 2, 2, 2, 2, 2, 2, 2, 2, 2, 2, 2, 2, 2, 2, 2, 2, 2, 2, 2, 2, 2, 2, 2, 2, 2, 2, 2, 2, 2, 2, 3 ),
 ( 0.000000000000000000, 1.000000000000000000 ),
 ( 0.000000000000000000, 0.01388888888888888812, 0.02777777777777777624, 0.04166666666666666435, 0.05555555555555555247, 0.06944444444444444753, 0.08333333333333332871, 0.09722222222222222376, 0.1111111111111111049, 0.1250000000000000000, 0.1388888888888888951, 0.1527777777777777901, 0.1666666666666666574, 0.1805555555555555525, 0.1944444444444444475, 0.2083333333333333426, 0.2222222222222222099, 0.2361111111111111049, 0.2500000000000000000, 0.2638888888888888951, 0.2777777777777777901, 0.2916666666666666852, 0.3055555555555555802, 0.3194444444444444198, 0.3333333333333333148, 0.3472222222222222099, 0.3611111111111111049, 0.3750000000000000000, 0.3888888888888888951, 0.4027777777777777901, 0.4166666666666666852, 0.4305555555555555802, 0.4444444444444444198, 0.4583333333333333148, 0.4722222222222222099, 0.4861111111111111049, 0.5000000000000000000, 0.5138888888888888395, 0.5277777777777777901, 0.5416666666666666297, 0.5555555555555555802, 0.5694444444444444198, 0.5833333333333333703, 0.5972222222222222099, 0.6111111111111111605, 0.6250000000000000000, 0.6388888888888888395, 0.6527777777777777901, 0.6666666666666666297, 0.6805555555555555802, 0.6944444444444444198, 0.7083333333333333703, 0.7222222222222222099, 0.7361111111111111605, 0.7500000000000000000, 0.7638888888888888395, 0.7777777777777777901, 0.7916666666666666297, 0.8055555555555555802, 0.8194444444444444198, 0.8333333333333333703, 0.8472222222222222099, 0.8611111111111111605, 0.8750000000000000000, 0.8888888888888888395, 0.9027777777777777901, 0.9166666666666666297, 0.9258784821878333071, 0.9351372670097116702 ),
 .UNSPECIFIED. ) 
 GEOMETRIC_REPRESENTATION_ITEM ( )  RATIONAL_B_SPLINE_SURFACE ( (
 ( 1.000000000000000000, 0.8660254037844387076, 1.000000000000000000, 0.8660254037844387076, 1.000000000000000000, 0.8660254037844387076, 1.000000000000000000, 0.8660254037844387076, 1.000000000000000000, 0.8660254037844387076, 1.000000000000000000, 0.8660254037844387076, 1.000000000000000000, 0.8660254037844387076, 1.000000000000000000, 0.8660254037844387076, 1.000000000000000000, 0.8660254037844387076, 1.000000000000000000, 0.8660254037844387076, 1.000000000000000000, 0.8660254037844387076, 1.000000000000000000, 0.8660254037844387076, 1.000000000000000000, 0.8660254037844387076, 1.000000000000000000, 0.8660254037844387076, 1.000000000000000000, 0.8660254037844387076, 1.000000000000000000, 0.8660254037844387076, 1.000000000000000000, 0.8660254037844387076, 1.000000000000000000, 0.8660254037844387076, 1.000000000000000000, 0.8660254037844387076, 1.000000000000000000, 0.8660254037844387076, 1.000000000000000000, 0.8660254037844387076, 1.000000000000000000, 0.8660254037844387076, 1.000000000000000000, 0.8660254037844387076, 1.000000000000000000, 0.8660254037844387076, 1.000000000000000000, 0.8660254037844387076, 1.000000000000000000, 0.8660254037844387076, 1.000000000000000000, 0.8660254037844387076, 1.000000000000000000, 0.8660254037844387076, 1.000000000000000000, 0.8660254037844387076, 1.000000000000000000, 0.8660254037844387076, 1.000000000000000000, 0.8660254037844387076, 1.000000000000000000, 0.8660254037844387076, 1.000000000000000000, 0.8660254037844387076, 1.000000000000000000, 0.8660254037844387076, 1.000000000000000000, 0.8660254037844387076, 1.000000000000000000, 0.8660254037844387076, 1.000000000000000000, 0.8660254037844387076, 1.000000000000000000, 0.8660254037844387076, 1.000000000000000000, 0.8660254037844387076, 1.000000000000000000, 0.8660254037844387076, 1.000000000000000000, 0.8660254037844387076, 1.000000000000000000, 0.8660254037844387076, 1.000000000000000000, 0.8660254037844387076, 1.000000000000000000, 0.8660254037844387076, 1.000000000000000000, 0.8660254037844387076, 1.000000000000000000, 0.8660254037844387076, 1.000000000000000000, 0.8660254037844387076, 1.000000000000000000, 0.8660254037844387076, 1.000000000000000000, 0.8660254037844387076, 1.000000000000000000, 0.8660254037844387076, 1.000000000000000000, 0.8660254037844387076, 1.000000000000000000, 0.8660254037844387076, 1.000000000000000000, 0.8660254037844387076, 1.000000000000000000, 0.8660254037844387076, 1.000000000000000000, 0.8660254037844387076, 1.000000000000000000, 0.8660254037844387076, 1.000000000000000000, 0.8660254037844387076, 1.000000000000000000, 0.8660254037844387076, 1.000000000000000000, 0.8660254037844387076, 1.000000000000000000, 0.8660254037844387076, 1.000000000000000000, 0.8660254037844387076, 1.000000000000000000, 0.8660254037844387076, 1.000000000000000000, 0.8660254037844387076, 1.000000000000000000, 0.8660254037844387076, 1.000000000000000000, 0.8660254037844387076, 1.000000000000000000, 0.8660254037844387076, 1.000000000000000000, 0.9111412529300411123, 0.9401537613649495473, 0.9401537613649495473, 0.9401537613649495473),
 ( 1.000000000000000000, 0.8660254037844387076, 1.000000000000000000, 0.8660254037844387076, 1.000000000000000000, 0.8660254037844387076, 1.000000000000000000, 0.8660254037844387076, 1.000000000000000000, 0.8660254037844387076, 1.000000000000000000, 0.8660254037844387076, 1.000000000000000000, 0.8660254037844387076, 1.000000000000000000, 0.8660254037844387076, 1.000000000000000000, 0.8660254037844387076, 1.000000000000000000, 0.8660254037844387076, 1.000000000000000000, 0.8660254037844387076, 1.000000000000000000, 0.8660254037844387076, 1.000000000000000000, 0.8660254037844387076, 1.000000000000000000, 0.8660254037844387076, 1.000000000000000000, 0.8660254037844387076, 1.000000000000000000, 0.8660254037844387076, 1.000000000000000000, 0.8660254037844387076, 1.000000000000000000, 0.8660254037844387076, 1.000000000000000000, 0.8660254037844387076, 1.000000000000000000, 0.8660254037844387076, 1.000000000000000000, 0.8660254037844387076, 1.000000000000000000, 0.8660254037844387076, 1.000000000000000000, 0.8660254037844387076, 1.000000000000000000, 0.8660254037844387076, 1.000000000000000000, 0.8660254037844387076, 1.000000000000000000, 0.8660254037844387076, 1.000000000000000000, 0.8660254037844387076, 1.000000000000000000, 0.8660254037844387076, 1.000000000000000000, 0.8660254037844387076, 1.000000000000000000, 0.8660254037844387076, 1.000000000000000000, 0.8660254037844387076, 1.000000000000000000, 0.8660254037844387076, 1.000000000000000000, 0.8660254037844387076, 1.000000000000000000, 0.8660254037844387076, 1.000000000000000000, 0.8660254037844387076, 1.000000000000000000, 0.8660254037844387076, 1.000000000000000000, 0.8660254037844387076, 1.000000000000000000, 0.8660254037844387076, 1.000000000000000000, 0.8660254037844387076, 1.000000000000000000, 0.8660254037844387076, 1.000000000000000000, 0.8660254037844387076, 1.000000000000000000, 0.8660254037844387076, 1.000000000000000000, 0.8660254037844387076, 1.000000000000000000, 0.8660254037844387076, 1.000000000000000000, 0.8660254037844387076, 1.000000000000000000, 0.8660254037844387076, 1.000000000000000000, 0.8660254037844387076, 1.000000000000000000, 0.8660254037844387076, 1.000000000000000000, 0.8660254037844387076, 1.000000000000000000, 0.8660254037844387076, 1.000000000000000000, 0.8660254037844387076, 1.000000000000000000, 0.8660254037844387076, 1.000000000000000000, 0.8660254037844387076, 1.000000000000000000, 0.8660254037844387076, 1.000000000000000000, 0.8660254037844387076, 1.000000000000000000, 0.8660254037844387076, 1.000000000000000000, 0.8660254037844387076, 1.000000000000000000, 0.8660254037844387076, 1.000000000000000000, 0.8660254037844387076, 1.000000000000000000, 0.8660254037844387076, 1.000000000000000000, 0.8660254037844387076, 1.000000000000000000, 0.8660254037844387076, 1.000000000000000000, 0.8660254037844387076, 1.000000000000000000, 0.8660254037844387076, 1.000000000000000000, 0.8660254037844387076, 1.000000000000000000, 0.8660254037844387076, 1.000000000000000000, 0.9111412529300411123, 0.9401537613649495473, 0.9401537613649495473, 0.9401537613649495473) ) ) 
 REPRESENTATION_ITEM ( '' )  SURFACE ( )  );
#6266 = EDGE_LOOP ( 'NONE', ( #8434, #7945, #5263, #6393 ) ) ;
#6267 = CARTESIAN_POINT ( 'NONE',  ( 9.063633472794011325, 99.49999999999998579, 19.59517414759687526 ) ) ;
#6268 = CARTESIAN_POINT ( 'NONE',  ( 1.128215178124999607, -0.7406249993854829849, -1.954126010382871259 ) ) ;
#6269 = ADVANCED_FACE ( 'NONE', ( #6426 ), #4650, .T. ) ;
#6270 = B_SPLINE_SURFACE_WITH_KNOTS ( 'NONE', 3, 1, ( 
 ( #4603, #7795 ),
 ( #626, #3663 ),
 ( #4493, #10038 ),
 ( #2197, #2874 ),
 ( #6006, #1249 ),
 ( #3825, #4439 ),
 ( #9199, #3714 ),
 ( #6058, #9425 ),
 ( #467, #6897 ),
 ( #9307, #2139 ),
 ( #7741, #574 ),
 ( #3768, #734 ),
 ( #9673, #8053 ),
 ( #6335, #8889 ),
 ( #6432, #7211 ) ),
 .UNSPECIFIED., .F., .F., .F.,
 ( 4, 1, 1, 1, 1, 1, 1, 1, 1, 1, 1, 1, 4 ),
 ( 2, 2 ),
 ( 0.000000000000000000, 0.08963690308348271074, 0.1775767702671464110, 0.2649576542713044658, 0.3533131777157214604, 0.4402865524342069459, 0.5245518675747646853, 0.6066224975438009315, 0.6889424263984335051, 0.7698335385027974542, 0.8475882324521423206, 0.9236428641877653112, 1.000000000000000000 ),
 ( 0.000000000000000000, 1.000000000000000000 ),
 .UNSPECIFIED. ) ;
#6271 = ORIENTED_EDGE ( 'NONE', *, *, #8965, .T. ) ;
#6272 = FACE_OUTER_BOUND ( 'NONE', #3230, .T. ) ;
#6273 = CARTESIAN_POINT ( 'NONE',  ( 9.778118981323553172, 99.49999999999998579, 20.11889122584574352 ) ) ;
#6274 = EDGE_CURVE ( 'NONE', #3142, #2494, #3791, .T. ) ;
#6275 = CARTESIAN_POINT ( 'NONE',  ( 4.996790860652426159E-15, -1.856249998770965748, -2.500000000000000000 ) ) ;
#6276 = ORIENTED_EDGE ( 'NONE', *, *, #911, .T. ) ;
#6277 = CARTESIAN_POINT ( 'NONE',  ( -14.76042637754942177, 99.50000000000000000, 16.05242888258284140 ) ) ;
#6278 = CARTESIAN_POINT ( 'NONE',  ( -27.43301270000000258, 3.099999998907525089, -11.36312591709336317 ) ) ;
#6279 = VERTEX_POINT ( 'NONE', #6216 ) ;
#6280 = CARTESIAN_POINT ( 'NONE',  ( 2.500000000000000000, -3.787499999999999645, -1.443375672974064994 ) ) ;
#6281 = TOROIDAL_SURFACE ( 'NONE', #4769, 23.82500000000000284, 1.324999999999999956 ) ;
#6282 = CARTESIAN_POINT ( 'NONE',  ( -0.6698729810778069060, -0.4861538093386316151, -2.500000000000000000 ) ) ;
#6283 = CARTESIAN_POINT ( 'NONE',  ( -2.256430356250000102, -0.1406249993854829794, 0.000000000000000000 ) ) ;
#6284 = CARTESIAN_POINT ( 'NONE',  ( -16.91659681606879317, 99.50000000000000000, 15.78485274883190392 ) ) ;
#6285 = CARTESIAN_POINT ( 'NONE',  ( -11.36312591709335962, 3.799999998907525711, -27.43301270000000258 ) ) ;
#6286 = CARTESIAN_POINT ( 'NONE',  ( -15.19031985176477662, 99.99999999999995737, 15.56880617076518547 ) ) ;
#6287 = CARTESIAN_POINT ( 'NONE',  ( 26.99999999999999645, 3.749999997815050445, 11.18376618407358691 ) ) ;
#6288 = CARTESIAN_POINT ( 'NONE',  ( 2.901827748664965068, 99.49999999999998579, -21.68759887446373469 ) ) ;
#6289 = EDGE_CURVE ( 'NONE', #3656, #7920, #3863, .T. ) ;
#6290 = CARTESIAN_POINT ( 'NONE',  ( -4.959819536546781389E-15, 3.799999999999999822, 27.00000000000000355 ) ) ;
#6291 = CARTESIAN_POINT ( 'NONE',  ( 2.256430356250000546, -4.903124999385481964, 1.302750673588579877 ) ) ;
#6292 = CARTESIAN_POINT ( 'NONE',  ( 4.118246196500586542, 99.49999999999998579, -21.10643963665684453 ) ) ;
#6293 = ORIENTED_EDGE ( 'NONE', *, *, #385, .T. ) ;
#6294 = CARTESIAN_POINT ( 'NONE',  ( 1.128215178124999607, -2.540624999385482585, -1.954126010382871259 ) ) ;
#6295 = CARTESIAN_POINT ( 'NONE',  ( 27.43301270000000258, 5.099999998907525978, -11.36312591709336139 ) ) ;
#6296 =( LENGTH_UNIT ( ) NAMED_UNIT ( * ) SI_UNIT ( .MILLI., .METRE. ) );
#6297 = CARTESIAN_POINT ( 'NONE',  ( -15.56505537928961047, 99.99999999999998579, 14.87309967080592088 ) ) ;
#6298 = MANIFOLD_SOLID_BREP ( 'Boss-Extrude1', #8814 ) ;
#6299 = CARTESIAN_POINT ( 'NONE',  ( -19.09188309203678457, 2.700000000000000178, -19.09188309203678813 ) ) ;
#6300 = CARTESIAN_POINT ( 'NONE',  ( 8.829292973371666520, 99.49999999999998579, 19.92220432019063736 ) ) ;
#6301 = ORIENTED_EDGE ( 'NONE', *, *, #5449, .F. ) ;
#6302 = VERTEX_POINT ( 'NONE', #9521 ) ;
#6303 = VECTOR ( 'NONE', #4988, 1000.000000000000000 ) ;
#6304 = CARTESIAN_POINT ( 'NONE',  ( -15.30604604128650692, 99.50000000000000000, 15.41317891555018349 ) ) ;
#6305 = CARTESIAN_POINT ( 'NONE',  ( 8.081885929396888102, 99.50000000000001421, 20.89785832093561169 ) ) ;
#6306 = ORIENTED_EDGE ( 'NONE', *, *, #5829, .F. ) ;
#6307 = CARTESIAN_POINT ( 'NONE',  ( -1.128215178125000273, -3.478124999385482141, -1.954126010382871259 ) ) ;
#6308 = ORIENTED_EDGE ( 'NONE', *, *, #7485, .F. ) ;
#6309 = CARTESIAN_POINT ( 'NONE',  ( -27.43301270000000969, 3.099999998907525089, 11.36312591709335784 ) ) ;
#6310 = CARTESIAN_POINT ( 'NONE',  ( -21.13452028402337035, 99.50000000000000000, -9.824917503107416294 ) ) ;
#6311 = B_SPLINE_CURVE_WITH_KNOTS ( 'NONE', 3,
 ( #6483, #7058, #10314, #3151, #9529, #3245, #101, #2511, #2353, #9573, #837, #2305, #4078, #5550, #5702, #1714, #8107, #8005, #4910 ),
 .UNSPECIFIED., .F., .F.,
 ( 4, 1, 1, 1, 1, 1, 1, 1, 1, 1, 1, 1, 1, 1, 1, 1, 4 ),
 ( 0.000000000000000000, 0.06455295689170470474, 0.1273249605695649933, 0.1891299628201091876, 0.2499617887110622549, 0.3104215510145779122, 0.3717966107350694216, 0.4346754705585744727, 0.4991966429079077727, 0.5636107885140392293, 0.6264421791528413941, 0.6882713145562978641, 0.7491215306807221808, 0.8100115732567139126, 0.8716292230916812267, 0.9349778748807419104, 1.000000000000000000 ),
 .UNSPECIFIED. ) ;
#6312 = AXIS2_PLACEMENT_3D ( 'NONE', #1349, #1243, #675 ) ;
#6313 = VECTOR ( 'NONE', #188, 1000.000000000000000 ) ;
#6314 = CARTESIAN_POINT ( 'NONE',  ( 1.128215178124999607, -0.8531249993854828073, -1.954126010382871259 ) ) ;
#6315 = DIRECTION ( 'NONE',  ( 0.3918949146621865109, 0.000000000000000000, 0.9200099868272720860 ) ) ;
#6316 = ORIENTED_EDGE ( 'NONE', *, *, #8891, .T. ) ;
#6317 = DIRECTION ( 'NONE',  ( 0.000000000000000000, -1.000000000000000000, 0.000000000000000000 ) ) ;
#6318 = AXIS2_PLACEMENT_3D ( 'NONE', #4344, #6748, #9109 ) ;
#6319 = CARTESIAN_POINT ( 'NONE',  ( -2.500000000000000000, -2.681249998770965259, -1.443375672974064106 ) ) ;
#6320 = CARTESIAN_POINT ( 'NONE',  ( 1.045839947578414805E-15, -0.9562499987709659477, -2.500000000000000000 ) ) ;
#6321 = CARTESIAN_POINT ( 'NONE',  ( -16.07368679829020763, 99.50000000000000000, 17.11560437002838952 ) ) ;
#6322 = DIRECTION ( 'NONE',  ( -0.000000000000000000, 1.000000000000000000, -0.000000000000000000 ) ) ;
#6323 = CARTESIAN_POINT ( 'NONE',  ( 1.128215178125001161, -1.340624999385482852, 1.954126010382870815 ) ) ;
#6324 = ADVANCED_FACE ( 'NONE', ( #1559 ), #10360, .F. ) ;
#6325 = CARTESIAN_POINT ( 'NONE',  ( -16.49187002848391970, 99.50000000000001421, 16.71294888518108124 ) ) ;
#6326 = VECTOR ( 'NONE', #10272, 1000.000000000000227 ) ;
#6327 =( BOUNDED_CURVE ( )  B_SPLINE_CURVE ( 2, ( #7926, #7188, #3358, #4102, #9739 ),
 .UNSPECIFIED., .F., .T. ) 
 B_SPLINE_CURVE_WITH_KNOTS ( ( 3, 2, 3 ),
 ( 0.000000000000000000, 0.01785714285714285615, 0.03571428571428571230 ),
 .UNSPECIFIED. ) 
 CURVE ( )  GEOMETRIC_REPRESENTATION_ITEM ( )  RATIONAL_B_SPLINE_CURVE ( ( 1.000000000000000000, 0.9238795325112867385, 1.000000000000000000, 0.9238795325112867385, 1.000000000000000000 ) ) 
 REPRESENTATION_ITEM ( '' )  );
#6328 = CARTESIAN_POINT ( 'NONE',  ( -22.29247428061501779, 99.50000000000000000, -10.66603791136541624 ) ) ;
#6329 = CARTESIAN_POINT ( 'NONE',  ( -16.36254897777739004, 100.0000000000000142, 15.39785597259249350 ) ) ;
#6330 = CARTESIAN_POINT ( 'NONE',  ( 11.36312591709336139, 3.699999998907525622, -27.43301270000000258 ) ) ;
#6331 = ORIENTED_EDGE ( 'NONE', *, *, #1547, .F. ) ;
#6332 = CARTESIAN_POINT ( 'NONE',  ( 2.500000000000000000, -4.687500000000000000, -1.443375672974064994 ) ) ;
#6333 = B_SPLINE_CURVE_WITH_KNOTS ( 'NONE', 3,
 ( #8375, #7426, #1981, #9060, #5969, #8961, #5913, #9946, #5071, #5023, #1053, #4245, #8273, #422, #318, #1779, #1205, #3562, #5125 ),
 .UNSPECIFIED., .F., .F.,
 ( 4, 1, 1, 1, 1, 1, 1, 1, 1, 1, 1, 1, 1, 1, 1, 1, 4 ),
 ( 0.000000000000000000, 0.06839333837245492598, 0.1346519561570838353, 0.1985335841112251809, 0.2613354512981445610, 0.3228799447584090876, 0.3842093944964607433, 0.4462111754260434937, 0.5089246482083435996, 0.5715029624870164859, 0.6324491702983550123, 0.6923675070709934820, 0.7521785462597534444, 0.8119602890481165680, 0.8728645645504365946, 0.9355733815441056311, 1.000000000000000000 ),
 .UNSPECIFIED. ) ;
#6334 = ITEM_DEFINED_TRANSFORMATION ( 'NONE', 'NONE', #9657,  #5055 ) ;
#6335 = CARTESIAN_POINT ( 'NONE',  ( 2.847408871211157155, 99.50000000000001421, -22.10537533382872510 ) ) ;
#6336 = CARTESIAN_POINT ( 'NONE',  ( -2.256430356250000102, -3.403124999385482408, 0.000000000000000000 ) ) ;
#6337 = CARTESIAN_POINT ( 'NONE',  ( -21.18296228862668329, 99.50000000000002842, -10.95406920104765724 ) ) ;
#6338 = CARTESIAN_POINT ( 'NONE',  ( -19.09188309203678813, 1.899999997815050579, 19.09188309203678457 ) ) ;
#6339 = DIRECTION ( 'NONE',  ( 0.5074415416931677969, 0.000000000000000000, 0.8616861851997287269 ) ) ;
#6340 = CARTESIAN_POINT ( 'NONE',  ( 3.320270046935387853, 99.99999999999998579, -23.88810568987970484 ) ) ;
#6341 = CARTESIAN_POINT ( 'NONE',  ( 3.552835461024879127, 99.50000000000000000, -21.47801279722421697 ) ) ;
#6342 = CARTESIAN_POINT ( 'NONE',  ( 19.09188309203678102, 3.900000000000000355, 19.09188309203678813 ) ) ;
#6343 = CARTESIAN_POINT ( 'NONE',  ( -1.595409442497313560E-16, -3.403124999385482408, -2.605501347177161087 ) ) ;
#6344 = CARTESIAN_POINT ( 'NONE',  ( 3.861186820804014097, 99.50000000000004263, -21.07288982789904708 ) ) ;
#6345 = ORIENTED_EDGE ( 'NONE', *, *, #4146, .T. ) ;
#6346 = CARTESIAN_POINT ( 'NONE',  ( -1.128215178124998497, -2.765624999385482674, 1.954126010382872147 ) ) ;
#6347 = CARTESIAN_POINT ( 'NONE',  ( -19.39806930854668465, 4.749999998907525445, 19.39806930854667755 ) ) ;
#6348 = EDGE_CURVE ( 'NONE', #4897, #9070, #8098, .T. ) ;
#6349 = DIRECTION ( 'NONE',  ( 0.000000000000000000, -1.000000000000000000, 0.000000000000000000 ) ) ;
#6350 = EDGE_CURVE ( 'NONE', #393, #4830, #3421, .T. ) ;
#6351 = CARTESIAN_POINT ( 'NONE',  ( 26.99999999999999645, 3.950000000000000178, 11.18376618407358691 ) ) ;
#6352 = CARTESIAN_POINT ( 'NONE',  ( 2.500000000000000444, -3.356249998770965082, 1.443375672974063439 ) ) ;
#6353 = ORIENTED_EDGE ( 'NONE', *, *, #7297, .F. ) ;
#6354 = DIRECTION ( 'NONE',  ( -0.000000000000000000, -1.000000000000000000, -0.000000000000000000 ) ) ;
#6355 = CARTESIAN_POINT ( 'NONE',  ( -15.76250887235353737, 99.49999999999998579, 16.65066592061022277 ) ) ;
#6356 = CARTESIAN_POINT ( 'NONE',  ( -2.256430356250000102, -4.753124999385482496, 0.000000000000000000 ) ) ;
#6357 = CARTESIAN_POINT ( 'NONE',  ( -20.74358258379034936, 99.99999999999992895, -9.818556592845180120 ) ) ;
#6358 = CARTESIAN_POINT ( 'NONE',  ( 1.679787559701184688E-15, 3.649999998907525356, -27.43301270000000258 ) ) ;
#6359 = CARTESIAN_POINT ( 'NONE',  ( 3.097283534322414766, 99.50000000000002842, -24.18405864774921454 ) ) ;
#6360 = B_SPLINE_SURFACE_WITH_KNOTS ( 'NONE', 3, 1, ( 
 ( #3012, #6189 ),
 ( #6079, #5298 ),
 ( #4829, #8906 ),
 ( #2529, #1733 ),
 ( #5721, #805 ),
 ( #1636, #9545 ),
 ( #997, #4969 ),
 ( #2572, #2369 ),
 ( #3999, #7182 ),
 ( #165, #5568 ),
 ( #6452, #6500 ) ),
 .UNSPECIFIED., .F., .F., .F.,
 ( 4, 1, 1, 1, 1, 1, 1, 1, 4 ),
 ( 2, 2 ),
 ( 0.000000000000000000, 0.1243175037779491315, 0.2437391319546453605, 0.3610119291759345539, 0.4796059399169178006, 0.5994854737745749507, 0.7252340722053824962, 0.8585022233306516259, 1.000000000000000000 ),
 ( 0.000000000000000000, 1.000000000000000000 ),
 .UNSPECIFIED. ) ;
#6361 = CARTESIAN_POINT ( 'NONE',  ( 2.500000000000000000, -1.087499999999999911, -1.443375672974065438 ) ) ;
#6362 = CARTESIAN_POINT ( 'NONE',  ( 2.256430356250000546, -2.765624999385482674, 1.302750673588579877 ) ) ;
#6363 = CARTESIAN_POINT ( 'NONE',  ( 1.653273178848927064E-15, 1.599999997815050312, -27.00000000000000355 ) ) ;
#6364 = CARTESIAN_POINT ( 'NONE',  ( -16.76168403648438243, 100.0000000000000284, 16.44483764528499847 ) ) ;
#6365 = CARTESIAN_POINT ( 'NONE',  ( 4.363164797760430424, 100.0000000000000000, -21.67376679147534446 ) ) ;
#6366 = CARTESIAN_POINT ( 'NONE',  ( -2.500000000000000000, -2.193749998770965881, 0.000000000000000000 ) ) ;
#6367 = VECTOR ( 'NONE', #5208, 1000.000000000000000 ) ;
#6368 = LINE ( 'NONE', #9562, #1280 ) ;
#6369 = CARTESIAN_POINT ( 'NONE',  ( -0.6698729810778054627, -3.057596189432333578, 2.500000000000000000 ) ) ;
#6370 = DIRECTION ( 'NONE',  ( 0.000000000000000000, 0.000000000000000000, -1.000000000000000000 ) ) ;
#6371 = CARTESIAN_POINT ( 'NONE',  ( 2.256430356250000102, -4.865624999385482319, -2.763330213280484622E-16 ) ) ;
#6372 = CARTESIAN_POINT ( 'NONE',  ( -22.35673484330673944, 100.0000000000000142, -10.41320610523044721 ) ) ;
#6373 = LINE ( 'NONE', #2346, #7654 ) ;
#6374 = DIRECTION ( 'NONE',  ( -0.9985315370676780544, 0.000000000000000000, 0.05417351272771728232 ) ) ;
#6375 = CARTESIAN_POINT ( 'NONE',  ( 1.679787559701184688E-15, 3.749999998907525445, -27.43301270000000258 ) ) ;
#6376 = ORIENTED_EDGE ( 'NONE', *, *, #5491, .F. ) ;
#6377 = EDGE_CURVE ( 'NONE', #1366, #4987, #9807, .T. ) ;
#6378 = CARTESIAN_POINT ( 'NONE',  ( 1.250000000000001110, -4.349999999999999645, 2.165063509461096380 ) ) ;
#6379 = ADVANCED_BREP_SHAPE_REPRESENTATION ( '', ( #6220, #5055 ), #1396 ) ;
#6380 = CARTESIAN_POINT ( 'NONE',  ( 3.275092494823534928, 99.50000000000000000, -23.54688978826290580 ) ) ;
#6381 = CARTESIAN_POINT ( 'NONE',  ( -1.128215178124998497, -3.778124999385482408, 1.954126010382872147 ) ) ;
#6382 = CARTESIAN_POINT ( 'NONE',  ( -21.07003209069497984, 99.99999999999998579, -11.28505157174820361 ) ) ;
#6383 = CARTESIAN_POINT ( 'NONE',  ( -4.959819536546781389E-15, 1.999999997815050445, 27.00000000000000355 ) ) ;
#6384 =( BOUNDED_CURVE ( )  B_SPLINE_CURVE ( 2, ( #6696, #5130, #9791, #8382, #5074, #3626, #9211, #2043, #1934 ),
 .UNSPECIFIED., .F., .T. ) 
 B_SPLINE_CURVE_WITH_KNOTS ( ( 3, 2, 2, 2, 3 ),
 ( 0.8214285714285713969, 0.8392857142857143016, 0.8571428571428570953, 0.8750000000000000000, 0.8928571428571429047 ),
 .UNSPECIFIED. ) 
 CURVE ( )  GEOMETRIC_REPRESENTATION_ITEM ( )  RATIONAL_B_SPLINE_CURVE ( ( 1.000000000000000000, 0.9238795325112867385, 1.000000000000000000, 0.9238795325112867385, 1.000000000000000000, 0.9238795325112867385, 1.000000000000000000, 0.9238795325112867385, 1.000000000000000000 ) ) 
 REPRESENTATION_ITEM ( '' )  );
#6385 = CARTESIAN_POINT ( 'NONE',  ( -15.18657300206754179, 99.99999999999997158, 16.26161032743331347 ) ) ;
#6386 = CARTESIAN_POINT ( 'NONE',  ( 9.342627931057743140, 100.0000000000000000, 21.59831790269294771 ) ) ;
#6387 = CARTESIAN_POINT ( 'NONE',  ( 3.317038232150706367, 99.99999999999998579, -21.66195598387956878 ) ) ;
#6388 = VECTOR ( 'NONE', #8314, 1000.000000000000000 ) ;
#6389 = FACE_OUTER_BOUND ( 'NONE', #5251, .T. ) ;
#6390 = CARTESIAN_POINT ( 'NONE',  ( 1.128215178125001161, -4.490624999385482319, 1.954126010382870815 ) ) ;
#6391 = CARTESIAN_POINT ( 'NONE',  ( 4.232798786556307036, 99.50000000000000000, -24.34936571594186105 ) ) ;
#6392 = EDGE_LOOP ( 'NONE', ( #1706, #3924, #6583, #9466 ) ) ;
#6393 = ORIENTED_EDGE ( 'NONE', *, *, #2486, .T. ) ;
#6394 = CARTESIAN_POINT ( 'NONE',  ( -1.128215178124998497, -1.865624999385482763, 1.954126010382872147 ) ) ;
#6395 = EDGE_CURVE ( 'NONE', #6501, #6993, #4486, .T. ) ;
#6396 = CARTESIAN_POINT ( 'NONE',  ( 27.43301270000000258, 1.199999998907525178, -11.36312591709336139 ) ) ;
#6397 =( NAMED_UNIT ( * ) SI_UNIT ( $, .STERADIAN. ) SOLID_ANGLE_UNIT ( ) );
#6398 = CARTESIAN_POINT ( 'NONE',  ( -15.34367147589386349, 99.50000000000004263, 16.87599331055909602 ) ) ;
#6399 = CARTESIAN_POINT ( 'NONE',  ( -19.39806930854668465, 0.7499999989075252227, 19.39806930854667755 ) ) ;
#6400 = CARTESIAN_POINT ( 'NONE',  ( 3.079986699855593473E-15, 85.00000000000000000, 25.15000000000000213 ) ) ;
#6401 = DIRECTION ( 'NONE',  ( 0.000000000000000000, -1.000000000000000000, 0.000000000000000000 ) ) ;
#6402 = CARTESIAN_POINT ( 'NONE',  ( -20.89884294283097432, 99.50000000000001421, -10.47119744953613640 ) ) ;
#6403 = EDGE_CURVE ( 'NONE', #9797, #2280, #978, .T. ) ;
#6404 = CARTESIAN_POINT ( 'NONE',  ( -2.256430356250000102, -3.440624999385482496, -1.302750673588580321 ) ) ;
#6405 = CARTESIAN_POINT ( 'NONE',  ( 1.034219503716432668E-14, -5.006249998770964993, -2.500000000000000000 ) ) ;
#6406 = AXIS2_PLACEMENT_3D ( 'NONE', #6580, #7267, #9771 ) ;
#6407 = ADVANCED_FACE ( 'NONE', ( #1069, #3374 ), #9026, .T. ) ;
#6408 = CARTESIAN_POINT ( 'NONE',  ( 27.43301270000000258, 1.099999998907525312, -11.36312591709336139 ) ) ;
#6409 = CARTESIAN_POINT ( 'NONE',  ( 3.350143586568126164, 100.0000000000000142, -24.46212657588250394 ) ) ;
#6410 = CARTESIAN_POINT ( 'NONE',  ( -11.18376618407356737, 0.8499999978150503122, -27.00000000000000355 ) ) ;
#6411 = CARTESIAN_POINT ( 'NONE',  ( -2.256430356250000102, -4.753124999385482496, 0.000000000000000000 ) ) ;
#6412 = CARTESIAN_POINT ( 'NONE',  ( -16.45635306197508996, 100.0000000000000000, 15.51056558312563105 ) ) ;
#6413 = ADVANCED_FACE ( 'NONE', ( #9080 ), #4264, .T. ) ;
#6414 = CARTESIAN_POINT ( 'NONE',  ( -22.58826642033182353, 99.49999999999998579, -9.883148377786627137 ) ) ;
#6415 = DIRECTION ( 'NONE',  ( 0.000000000000000000, 0.000000000000000000, -1.000000000000000000 ) ) ;
#6416 = B_SPLINE_CURVE_WITH_KNOTS ( 'NONE', 3,
 ( #3874, #7629, #526, #2199, #8532, #8477, #10268, #1468, #6116, #3100, #5454 ),
 .UNSPECIFIED., .F., .F.,
 ( 4, 1, 1, 1, 1, 1, 1, 1, 4 ),
 ( 0.000000000000000000, 0.1514666391271576040, 0.2940212016997327260, 0.4289076436562640482, 0.5568069201790899481, 0.6759213874835566793, 0.7888117551744765477, 0.8972989960681465593, 1.000000000000000000 ),
 .UNSPECIFIED. ) ;
#6417 = CARTESIAN_POINT ( 'NONE',  ( 1.250000000000001110, -3.393749998770965615, 2.165063509461096380 ) ) ;
#6418 = EDGE_CURVE ( 'NONE', #2954, #3286, #4856, .T. ) ;
#6419 = CARTESIAN_POINT ( 'NONE',  ( 4.523042264738025509, 99.50000000000001421, -24.25177047807976294 ) ) ;
#6420 = CARTESIAN_POINT ( 'NONE',  ( 0.000000000000000000, 0.000000000000000000, 0.000000000000000000 ) ) ;
#6421 = CARTESIAN_POINT ( 'NONE',  ( 9.445361748092775400, 99.50000000000001421, 19.75398588445988324 ) ) ;
#6422 = CARTESIAN_POINT ( 'NONE',  ( -2.256430356250000102, -5.090624999385482852, 0.000000000000000000 ) ) ;
#6423 = EDGE_LOOP ( 'NONE', ( #2221, #3505, #10214, #4000 ) ) ;
#6424 = CARTESIAN_POINT ( 'NONE',  ( -22.25406130147340633, 100.0000000000000284, -9.998337329044998611 ) ) ;
#6425 = EDGE_LOOP ( 'NONE', ( #9031, #4626, #8374, #5837 ) ) ;
#6426 = FACE_OUTER_BOUND ( 'NONE', #2161, .T. ) ;
#6427 = FACE_OUTER_BOUND ( 'NONE', #8772, .T. ) ;
#6428 = CARTESIAN_POINT ( 'NONE',  ( -16.34436021381890924, 100.0000000000000000, 15.38072013554846151 ) ) ;
#6429 = CARTESIAN_POINT ( 'NONE',  ( 11.36312591709336850, 4.999999998907526333, 27.43301269999999903 ) ) ;
#6430 = ORIENTED_EDGE ( 'NONE', *, *, #9006, .T. ) ;
#6431 = CARTESIAN_POINT ( 'NONE',  ( 3.207968951880266761, 99.49999999999998579, -22.92616835434091627 ) ) ;
#6432 = CARTESIAN_POINT ( 'NONE',  ( 2.852289972453743161, 99.50000000000000000, -22.14293542748032451 ) ) ;
#6433 = CARTESIAN_POINT ( 'NONE',  ( 4.786228327491941173E-16, -3.740624999385482319, 2.605501347177161087 ) ) ;
#6434 = CARTESIAN_POINT ( 'NONE',  ( -21.07003209069497984, 99.49999999999998579, -11.28505157174820361 ) ) ;
#6435 = CARTESIAN_POINT ( 'NONE',  ( -27.00000000000000355, 1.799999997815050490, -3.306546357697854128E-15 ) ) ;
#6436 = PRODUCT_DEFINITION_CONTEXT ( 'detailed design', #4600, 'design' ) ;
#6437 = DIRECTION ( 'NONE',  ( 0.000000000000000000, 0.000000000000000000, 1.000000000000000000 ) ) ;
#6438 = CARTESIAN_POINT ( 'NONE',  ( 3.296462644833695776, 100.0000000000000142, -23.81854410834942115 ) ) ;
#6439 = DIRECTION ( 'NONE',  ( 0.3368601548094422582, 0.000000000000000000, -0.9415546909775122097 ) ) ;
#6440 = PRODUCT_DEFINITION_SHAPE ( 'NONE', 'NONE',  #10371 ) ;
#6441 = LINE ( 'NONE', #10323, #1462 ) ;
#6442 = CARTESIAN_POINT ( 'NONE',  ( 1.128215178124999607, -3.890624999385482674, -1.954126010382871259 ) ) ;
#6443 = CARTESIAN_POINT ( 'NONE',  ( 3.428794695218988053, 99.50000000000001421, -24.07607503615978572 ) ) ;
#6444 = ORIENTED_EDGE ( 'NONE', *, *, #8074, .F. ) ;
#6445 = VECTOR ( 'NONE', #9731, 1000.000000000000000 ) ;
#6446 = EDGE_LOOP ( 'NONE', ( #8823, #5161, #2845, #335 ) ) ;
#6447 = CARTESIAN_POINT ( 'NONE',  ( 2.256430356250000102, -2.165624999385483029, -2.763330213280484622E-16 ) ) ;
#6448 = CARTESIAN_POINT ( 'NONE',  ( 27.43301270000000258, 4.249999998907525445, 0.000000000000000000 ) ) ;
#6449 = CARTESIAN_POINT ( 'NONE',  ( -15.45548338988150938, 99.49999999999997158, 16.93306818456458984 ) ) ;
#6450 = B_SPLINE_CURVE_WITH_KNOTS ( 'NONE', 3,
 ( #3502, #9884, #264, #6688, #1773, #9835, #2618 ),
 .UNSPECIFIED., .F., .F.,
 ( 4, 1, 1, 1, 4 ),
 ( 0.000000000000000000, 0.2676680225848128147, 0.5230972062070123885, 0.7658030722156558001, 1.000000000000000000 ),
 .UNSPECIFIED. ) ;
#6451 = CARTESIAN_POINT ( 'NONE',  ( 11.18376618407356915, 3.350000000000000089, -27.00000000000000355 ) ) ;
#6452 = CARTESIAN_POINT ( 'NONE',  ( 3.411785164761435674, 99.50000000000000000, -22.76693382491622231 ) ) ;
#6453 = EDGE_CURVE ( 'NONE', #7399, #5471, #5112, .T. ) ;
#6454 = CARTESIAN_POINT ( 'NONE',  ( 2.500000000000000444, -3.412500000000000089, 1.443375672974063439 ) ) ;
#6455 = CARTESIAN_POINT ( 'NONE',  ( -21.12798922145720582, 99.50000000000001421, -10.90888695829967325 ) ) ;
#6456 = AXIS2_PLACEMENT_3D ( 'NONE', #4060, #4159, #6415 ) ;
#6457 = ORIENTED_EDGE ( 'NONE', *, *, #6715, .T. ) ;
#6458 = CARTESIAN_POINT ( 'NONE',  ( 8.429066232339796017, 99.50000000000000000, 19.67794530653910101 ) ) ;
#6459 = ORIENTED_EDGE ( 'NONE', *, *, #8191, .T. ) ;
#6460 = CARTESIAN_POINT ( 'NONE',  ( -11.36312591709335962, 2.099999998907525089, -27.43301270000000258 ) ) ;
#6461 = CARTESIAN_POINT ( 'NONE',  ( 2.950788281418828429, 100.0000000000000142, -23.82341910423825837 ) ) ;
#6462 = CARTESIAN_POINT ( 'NONE',  ( 0.2187216588148096774, -20.00000000000000000, 3.085264589354759224 ) ) ;
#6463 = CARTESIAN_POINT ( 'NONE',  ( -2.256430356250000102, -2.990624999385482763, -1.302750673588580321 ) ) ;
#6464 = CARTESIAN_POINT ( 'NONE',  ( 0.000000000000000000, 97.00000000000000000, 0.000000000000000000 ) ) ;
#6465 = CARTESIAN_POINT ( 'NONE',  ( -22.43208371148383762, 99.50000000000000000, -9.654966607469265938 ) ) ;
#6466 = CARTESIAN_POINT ( 'NONE',  ( 4.772556553149396308, 99.99999999999997158, -24.49721679606612312 ) ) ;
#6467 = CARTESIAN_POINT ( 'NONE',  ( 2.500000000000000000, -4.668749998770964638, -3.061616997868383141E-16 ) ) ;
#6468 = ORIENTED_EDGE ( 'NONE', *, *, #6527, .F. ) ;
#6469 = VECTOR ( 'NONE', #1629, 1000.000000000000000 ) ;
#6470 = CARTESIAN_POINT ( 'NONE',  ( 2.500000000000000000, -1.031249998770965792, -1.443375672974065438 ) ) ;
#6471 = CARTESIAN_POINT ( 'NONE',  ( -20.63200021313574695, 99.50000000000000000, -10.19493994959453431 ) ) ;
#6472 = FACE_OUTER_BOUND ( 'NONE', #7703, .T. ) ;
#6473 = CARTESIAN_POINT ( 'NONE',  ( 4.786228327491941173E-16, -4.528124999385482852, 2.605501347177161087 ) ) ;
#6474 = EDGE_CURVE ( 'NONE', #2378, #3531, #145, .T. ) ;
#6475 = CLOSED_SHELL ( 'NONE', ( #6591, #4263, #8882, #7640, #8015, #5711, #2851, #3580, #7442, #638, #2360, #2861, #944, #6208, #3055 ) ) ;
#6476 = EDGE_CURVE ( 'NONE', #1992, #9410, #10362, .T. ) ;
#6477 = DIRECTION ( 'NONE',  ( 0.000000000000000000, -1.000000000000000000, 0.000000000000000000 ) ) ;
#6478 = CARTESIAN_POINT ( 'NONE',  ( -18.01369080470046313, 99.50000000000000000, 17.15556831233607937 ) ) ;
#6479 = CARTESIAN_POINT ( 'NONE',  ( 2.500000000000000000, -1.968749998770965792, -3.061616997868383141E-16 ) ) ;
#6480 = CARTESIAN_POINT ( 'NONE',  ( -11.36312591709337561, 3.299999998907525267, 27.43301269999999548 ) ) ;
#6481 = ORIENTED_EDGE ( 'NONE', *, *, #3915, .F. ) ;
#6482 = CARTESIAN_POINT ( 'NONE',  ( 3.949943451936506644, 99.50000000000000000, -21.41482314084395711 ) ) ;
#6483 = CARTESIAN_POINT ( 'NONE',  ( -20.96643530928959365, 99.99999999999997158, -10.05541671241504886 ) ) ;
#6484 = CARTESIAN_POINT ( 'NONE',  ( -1.595409442497313560E-16, -3.515624999385482674, -2.605501347177161087 ) ) ;
#6485 = CARTESIAN_POINT ( 'NONE',  ( 0.000000000000000000, 0.000000000000000000, 0.000000000000000000 ) ) ;
#6486 = CARTESIAN_POINT ( 'NONE',  ( -27.43301270000000258, 4.749999998907525445, -3.359575119402369376E-15 ) ) ;
#6487 = CARTESIAN_POINT ( 'NONE',  ( -15.11611088805441661, 99.50000000000000000, 16.06180012866831319 ) ) ;
#6488 = CARTESIAN_POINT ( 'NONE',  ( 3.286905236079108672, 99.50000000000004263, -23.77014634954566574 ) ) ;
#6489 = CARTESIAN_POINT ( 'NONE',  ( -9.703070624755296135E-15, -4.837500000000001243, 2.500000000000000444 ) ) ;
#6490 = CARTESIAN_POINT ( 'NONE',  ( -24.00000000000000711, 73.81339255365637086, 0.000000000000000000 ) ) ;
#6491 = CARTESIAN_POINT ( 'NONE',  ( 2.256430356250000546, -4.453124999385482674, 1.302750673588579877 ) ) ;
#6492 = CARTESIAN_POINT ( 'NONE',  ( 3.320270046935387853, 99.49999999999998579, -23.88810568987970484 ) ) ;
#6493 = VERTEX_POINT ( 'NONE', #6191 ) ;
#6494 = VERTEX_POINT ( 'NONE', #3527 ) ;
#6495 = CARTESIAN_POINT ( 'NONE',  ( 4.786228327491941173E-16, -4.078124999385482674, 2.605501347177161087 ) ) ;
#6496 = CARTESIAN_POINT ( 'NONE',  ( 27.43301270000000258, 5.049999998907525267, 0.000000000000000000 ) ) ;
#6497 = DIRECTION ( 'NONE',  ( 0.000000000000000000, 0.000000000000000000, 1.000000000000000000 ) ) ;
#6498 = CARTESIAN_POINT ( 'NONE',  ( 5.825495487346713297, 100.0000000000000000, 20.69456627699299744 ) ) ;
#6499 = CARTESIAN_POINT ( 'NONE',  ( 27.43301270000000258, 0.2499999989075252504, 0.000000000000000000 ) ) ;
#6500 = CARTESIAN_POINT ( 'NONE',  ( 3.411785164761435674, 100.0000000000000000, -22.76693382491622231 ) ) ;
#6501 = VERTEX_POINT ( 'NONE', #2162 ) ;
#6502 = CARTESIAN_POINT ( 'NONE',  ( 0.6698729810778025762, -3.467403810567665445, 2.500000000000002665 ) ) ;
#6503 = EDGE_LOOP ( 'NONE', ( #4719, #9007, #8399, #9849 ) ) ;
#6504 = CARTESIAN_POINT ( 'NONE',  ( 27.43301270000000258, 5.099999998907525089, -11.36312591709336139 ) ) ;
#6505 = CARTESIAN_POINT ( 'NONE',  ( 2.500000000000000444, -4.256249998770964993, 1.443375672974063439 ) ) ;
#6506 = EDGE_CURVE ( 'NONE', #6069, #7989, #3064, .T. ) ;
#6507 = CARTESIAN_POINT ( 'NONE',  ( -21.71039561923405969, 99.50000000000004263, -11.44438725057713313 ) ) ;
#6508 = CARTESIAN_POINT ( 'NONE',  ( 1.128215178124999607, -3.553124999385482319, -1.954126010382871259 ) ) ;
#6509 = DIRECTION ( 'NONE',  ( 0.2901787468363226652, 0.000000000000000000, 0.9569724629708534769 ) ) ;
#6510 = MECHANICAL_DESIGN_GEOMETRIC_PRESENTATION_REPRESENTATION (  '', ( #663 ), #1647 ) ;
#6511 = CARTESIAN_POINT ( 'NONE',  ( -22.59920249870969045, 99.49999999999998579, -10.80326527670058567 ) ) ;
#6512 = CARTESIAN_POINT ( 'NONE',  ( 8.149445629999579666, 100.0000000000000284, 20.33980848884064230 ) ) ;
#6513 = CARTESIAN_POINT ( 'NONE',  ( 2.500000000000000000, -4.218749998770966236, -3.061616997868383141E-16 ) ) ;
#6514 = ORIENTED_EDGE ( 'NONE', *, *, #4043, .F. ) ;
#6515 = CARTESIAN_POINT ( 'NONE',  ( -9.703070624755296135E-15, -5.231249998770965526, 2.500000000000000444 ) ) ;
#6516 = CARTESIAN_POINT ( 'NONE',  ( -20.69312081029678296, 99.49999999999997158, -9.926742041671966277 ) ) ;
#6517 = EDGE_CURVE ( 'NONE', #9173, #4212, #2644, .T. ) ;
#6518 = DIRECTION ( 'NONE',  ( -0.000000000000000000, -1.000000000000000000, -0.000000000000000000 ) ) ;
#6519 = CARTESIAN_POINT ( 'NONE',  ( -2.256430356250000102, -4.640624999385482674, 0.000000000000000000 ) ) ;
#6520 = ORIENTED_EDGE ( 'NONE', *, *, #4909, .F. ) ;
#6521 = CARTESIAN_POINT ( 'NONE',  ( -7.500000000000000000, 105.0000000000000142, -3.000000000000000000 ) ) ;
#6522 = LINE ( 'NONE', #5697, #5324 ) ;
#6523 = ADVANCED_FACE ( 'NONE', ( #5145 ), #8617, .T. ) ;
#6524 = CARTESIAN_POINT ( 'NONE',  ( -22.27115127098604574, 100.0000000000000000, -10.71048520281369676 ) ) ;
#6525 = CARTESIAN_POINT ( 'NONE',  ( 8.564701892180647036, 100.0000000000000000, 19.97971282122689018 ) ) ;
#6526 = ORIENTED_EDGE ( 'NONE', *, *, #1253, .T. ) ;
#6527 = EDGE_CURVE ( 'NONE', #3372, #3656, #5740, .T. ) ;
#6528 = DIRECTION ( 'NONE',  ( 0.000000000000000000, -1.000000000000000000, 0.000000000000000000 ) ) ;
#6529 = CARTESIAN_POINT ( 'NONE',  ( 2.971063225226878046, 99.50000000000000000, -23.91837856253154015 ) ) ;
#6530 = CARTESIAN_POINT ( 'NONE',  ( 8.051038018032482313, 99.99999999999994316, 19.92675698219059299 ) ) ;
#6531 = CARTESIAN_POINT ( 'NONE',  ( -20.52076770522338833, 100.0000000000000000, -10.69798695537560462 ) ) ;
#6532 = CARTESIAN_POINT ( 'NONE',  ( 11.18376618407356915, 0.7499999978150503344, -27.00000000000000355 ) ) ;
#6533 = CARTESIAN_POINT ( 'NONE',  ( -20.97746206809550884, 99.50000000000000000, -11.22189255051946688 ) ) ;
#6534 = ORIENTED_EDGE ( 'NONE', *, *, #181, .T. ) ;
#6535 = CARTESIAN_POINT ( 'NONE',  ( 1.250000000000001110, -4.743749998770965703, 2.165063509461096380 ) ) ;
#6536 = CARTESIAN_POINT ( 'NONE',  ( -16.11976138926855739, 99.49999999999997158, 16.60078749809536447 ) ) ;
#6537 = CARTESIAN_POINT ( 'NONE',  ( -21.44539290152690114, 99.50000000000000000, -11.08070480119962298 ) ) ;
#6538 = CARTESIAN_POINT ( 'NONE',  ( 3.486133158594717003E-16, -0.1125000000000000167, -2.500000000000000000 ) ) ;
#6539 = EDGE_LOOP ( 'NONE', ( #126, #862, #4089, #6681 ) ) ;
#6540 = ORIENTED_EDGE ( 'NONE', *, *, #1765, .T. ) ;
#6541 = CARTESIAN_POINT ( 'NONE',  ( -2.256430356250000102, -4.640624999385482674, 0.000000000000000000 ) ) ;
#6542 = CARTESIAN_POINT ( 'NONE',  ( 3.061616997868383141E-16, 0.000000000000000000, 2.500000000000000000 ) ) ;
#6543 = MANIFOLD_SOLID_BREP ( 'Thread1', #4135 ) ;
#6544 = CARTESIAN_POINT ( 'NONE',  ( 19.09188309203678102, 3.100000000000000533, 19.09188309203678813 ) ) ;
#6545 = DIRECTION ( 'NONE',  ( -0.000000000000000000, -1.000000000000000000, -0.000000000000000000 ) ) ;
#6546 = CYLINDRICAL_SURFACE ( 'NONE', #2940, 27.00000000000000355 ) ;
#6547 = CARTESIAN_POINT ( 'NONE',  ( 21.82251602564102910, 99.50000000000000000, -0.5181290064102563875 ) ) ;
#6548 = CARTESIAN_POINT ( 'NONE',  ( -20.89145576992255116, 99.49999999999997158, -10.33073932272468198 ) ) ;
#6549 = EDGE_LOOP ( 'NONE', ( #2959, #2275 ) ) ;
#6550 = ORIENTED_EDGE ( 'NONE', *, *, #3753, .F. ) ;
#6551 = CARTESIAN_POINT ( 'NONE',  ( 7.500000000000000000, 105.0000000000000142, 1.000000000000000222 ) ) ;
#6552 = CARTESIAN_POINT ( 'NONE',  ( 9.547662139763570366, 99.49999999999997158, 20.94662037603165672 ) ) ;
#6553 = AXIS2_PLACEMENT_3D ( 'NONE', #7601, #3524, #7441 ) ;
#6554 = CARTESIAN_POINT ( 'NONE',  ( -2.256430356249998770, -4.265624999385482674, 1.302750673588581876 ) ) ;
#6555 = CARTESIAN_POINT ( 'NONE',  ( -22.59920249870969045, 99.49999999999998579, -10.80326527670058567 ) ) ;
#6556 = CARTESIAN_POINT ( 'NONE',  ( -22.69331084068295112, 99.99999999999998579, -10.43328931840349050 ) ) ;
#6557 = CARTESIAN_POINT ( 'NONE',  ( -4.959819536546781389E-15, 5.199999997815050179, 27.00000000000000355 ) ) ;
#6558 = VECTOR ( 'NONE', #9974, 1000.000000000000000 ) ;
#6559 = EDGE_CURVE ( 'NONE', #7809, #4244, #3947, .T. ) ;
#6560 = CARTESIAN_POINT ( 'NONE',  ( -2.499999999999999556, -5.306249998770963927, 1.443375672974065882 ) ) ;
#6561 = ORIENTED_EDGE ( 'NONE', *, *, #8169, .T. ) ;
#6562 = CARTESIAN_POINT ( 'NONE',  ( -22.35642768247353729, 99.99999999999994316, -10.34293228154892752 ) ) ;
#6563 = CARTESIAN_POINT ( 'NONE',  ( 3.673732336774000018, 99.50000000000000000, -21.43557726391590279 ) ) ;
#6564 = CARTESIAN_POINT ( 'NONE',  ( 3.306546357697853733E-15, 5.000000000000000000, 27.00000000000000000 ) ) ;
#6565 = CARTESIAN_POINT ( 'NONE',  ( -2.256430356250000102, -3.778124999385482408, -1.302750673588580321 ) ) ;
#6566 = VECTOR ( 'NONE', #5248, 1000.000000000000000 ) ;
#6567 = CIRCLE ( 'NONE', #64, 27.00000000000000000 ) ;
#6568 = ADVANCED_FACE ( 'NONE', ( #7132 ), #8714, .T. ) ;
#6569 = EDGE_CURVE ( 'NONE', #2184, #3756, #7921, .T. ) ;
#6570 = CARTESIAN_POINT ( 'NONE',  ( 0.6698729810778087934, -1.482596189432334288, -2.499999999999999112 ) ) ;
#6571 = CARTESIAN_POINT ( 'NONE',  ( 3.673940397442059178E-15, 5.000000000000000000, 30.00000000000000000 ) ) ;
#6572 = CARTESIAN_POINT ( 'NONE',  ( 2.500000000000000000, -3.731249998770965970, -1.443375672974065438 ) ) ;
#6573 = ORIENTED_EDGE ( 'NONE', *, *, #8246, .T. ) ;
#6574 = CARTESIAN_POINT ( 'NONE',  ( 3.817429849879703241, 99.99999999999995737, -22.92346308580664171 ) ) ;
#6575 = CARTESIAN_POINT ( 'NONE',  ( 8.429066232339796017, 99.50000000000000000, 19.67794530653910101 ) ) ;
#6576 = CARTESIAN_POINT ( 'NONE',  ( 9.723125805078051798, 99.50000000000000000, 21.50134635983626907 ) ) ;
#6577 = CARTESIAN_POINT ( 'NONE',  ( -19.09188309203678457, 4.899999997815050357, -19.09188309203678813 ) ) ;
#6578 = DIRECTION ( 'NONE',  ( 0.9682498375925071565, 0.000000000000000000, 0.2499845035238856816 ) ) ;
#6579 = CARTESIAN_POINT ( 'NONE',  ( -21.24882413972086681, 99.50000000000002842, -9.742484589929601313 ) ) ;
#6580 = CARTESIAN_POINT ( 'NONE',  ( 0.000000000000000000, 0.000000000000000000, 0.000000000000000000 ) ) ;
#6581 = CARTESIAN_POINT ( 'NONE',  ( -21.51485068221570174, 100.0000000000000000, -11.09552232883975087 ) ) ;
#6582 = CARTESIAN_POINT ( 'NONE',  ( 2.500000000000000000, -4.724999999999998757, -3.061616997868383141E-16 ) ) ;
#6583 = ORIENTED_EDGE ( 'NONE', *, *, #5758, .T. ) ;
#6584 = VERTEX_POINT ( 'NONE', #67 ) ;
#6585 = CARTESIAN_POINT ( 'NONE',  ( -2.256430356249999214, -5.053124999385482319, 1.302750673588581876 ) ) ;
#6586 =( BOUNDED_CURVE ( )  B_SPLINE_CURVE ( 2, ( #2177, #8452, #1282, #7607, #3642, #4471, #5376, #501, #2119 ),
 .UNSPECIFIED., .F., .F. ) 
 B_SPLINE_CURVE_WITH_KNOTS ( ( 3, 2, 2, 2, 3 ),
 ( 0.1785714285714285754, 0.1964285714285714246, 0.2142857142857142738, 0.2321428571428571508, 0.2500000000000000000 ),
 .UNSPECIFIED. ) 
 CURVE ( )  GEOMETRIC_REPRESENTATION_ITEM ( )  RATIONAL_B_SPLINE_CURVE ( ( 1.000000000000000000, 0.9238795325112867385, 1.000000000000000000, 0.9238795325112867385, 1.000000000000000000, 0.9238795325112867385, 1.000000000000000000, 0.9238795325112867385, 1.000000000000000000 ) ) 
 REPRESENTATION_ITEM ( '' )  );
#6587 = CARTESIAN_POINT ( 'NONE',  ( -14.83571502646304197, 100.0000000000000284, 16.32397075880403392 ) ) ;
#6588 = CARTESIAN_POINT ( 'NONE',  ( 3.016803124593948393, 100.0000000000000142, -23.20507807535735978 ) ) ;
#6589 = CARTESIAN_POINT ( 'NONE',  ( 1.679787559701184688E-15, 1.249999998907525223, -27.43301270000000258 ) ) ;
#6590 = CARTESIAN_POINT ( 'NONE',  ( -2.499999999999999112, -0.8624999999999998224, 1.443375672974065882 ) ) ;
#6591 = ADVANCED_FACE ( 'NONE', ( #5621 ), #7283, .T. ) ;
#6592 = CARTESIAN_POINT ( 'NONE',  ( -23.82500000000000284, 72.50000000000001421, 0.000000000000000000 ) ) ;
#6593 = CARTESIAN_POINT ( 'NONE',  ( 0.000000000000000000, 5.000000000000004441, -27.00000000000000355 ) ) ;
#6594 = CARTESIAN_POINT ( 'NONE',  ( -20.99557965837879081, 99.99999999999994316, -10.74478602187354959 ) ) ;
#6595 = VECTOR ( 'NONE', #7613, 1000.000000000000000 ) ;
#6596 = ORIENTED_EDGE ( 'NONE', *, *, #512, .T. ) ;
#6597 = CARTESIAN_POINT ( 'NONE',  ( -21.79396932678589849, 99.99999999999994316, -9.306975108219608828 ) ) ;
#6598 = CARTESIAN_POINT ( 'NONE',  ( 2.950788281418828429, 100.0000000000000142, -23.82341910423825837 ) ) ;
#6599 = DIRECTION ( 'NONE',  ( -0.9572638942369904314, 0.000000000000000000, 0.2892158999609669712 ) ) ;
#6600 = CARTESIAN_POINT ( 'NONE',  ( -21.56977948371741505, 99.99999999999995737, -11.44450812306045329 ) ) ;
#6601 = CARTESIAN_POINT ( 'NONE',  ( 4.049441352997683374, 100.0000000000000000, -21.43849541167161732 ) ) ;
#6602 = CARTESIAN_POINT ( 'NONE',  ( -16.61132721736409934, 100.0000000000000142, 16.61681399495993716 ) ) ;
#6603 = VECTOR ( 'NONE', #9056, 1000.000000000000000 ) ;
#6604 = CARTESIAN_POINT ( 'NONE',  ( -1.728529299398585906, -5.253648441416169490, -1.450401466387756244 ) ) ;
#6605 = CARTESIAN_POINT ( 'NONE',  ( 5.098880966732203035, 100.0000000000000000, -24.13374913903897223 ) ) ;
#6606 = CARTESIAN_POINT ( 'NONE',  ( 5.302876193624534821E-16, -4.331249998770966059, 2.886751345948128655 ) ) ;
#6607 = ORIENTED_EDGE ( 'NONE', *, *, #5305, .F. ) ;
#6608 = ORIENTED_EDGE ( 'NONE', *, *, #9528, .T. ) ;
#6609 = CARTESIAN_POINT ( 'NONE',  ( -22.34867803760930727, 99.49999999999998579, -10.48295844864103721 ) ) ;
#6610 = CARTESIAN_POINT ( 'NONE',  ( 3.198738776810544415, 99.99999999999998579, -22.02447230026614022 ) ) ;
#6611 = CARTESIAN_POINT ( 'NONE',  ( -22.05902956123343017, 99.50000000000000000, -10.96257574645357558 ) ) ;
#6612 = FACE_OUTER_BOUND ( 'NONE', #8876, .T. ) ;
#6613 = CARTESIAN_POINT ( 'NONE',  ( 8.337740814200648387, 99.50000000000002842, 20.10843643765939248 ) ) ;
#6614 = VECTOR ( 'NONE', #1781, 1000.000000000000114 ) ;
#6615 = CARTESIAN_POINT ( 'NONE',  ( -2.500000000000000000, -3.600000000000000089, 0.000000000000000000 ) ) ;
#6616 = CARTESIAN_POINT ( 'NONE',  ( -19.09188309203678813, 2.699999997815051067, 19.09188309203678457 ) ) ;
#6617 = ORIENTED_EDGE ( 'NONE', *, *, #7012, .T. ) ;
#6618 = AXIS2_PLACEMENT_3D ( 'NONE', #9376, #687, #4668 ) ;
#6619 = CARTESIAN_POINT ( 'NONE',  ( 0.000000000000000000, -20.00000000000000000, 0.000000000000000000 ) ) ;
#6620 = ADVANCED_FACE ( 'NONE', ( #8810 ), #5522, .T. ) ;
#6621 = VECTOR ( 'NONE', #4170, 1000.000000000000000 ) ;
#6622 = CARTESIAN_POINT ( 'NONE',  ( 4.061354557346970040, 99.49999999999997158, -22.84864678426182039 ) ) ;
#6623 = CARTESIAN_POINT ( 'NONE',  ( 7.978247738654171251, 99.50000000000000000, 20.00924965157036794 ) ) ;
#6624 = ORIENTED_EDGE ( 'NONE', *, *, #4405, .F. ) ;
#6625 = CARTESIAN_POINT ( 'NONE',  ( 9.766630880609509902, 99.50000000000002842, 21.37293705761699059 ) ) ;
#6626 = CARTESIAN_POINT ( 'NONE',  ( 26.99999999999999645, 4.549999997815051600, 11.18376618407358691 ) ) ;
#6627 = DIRECTION ( 'NONE',  ( -0.3923379498508065000, 0.000000000000000000, -0.9198211419112228837 ) ) ;
#6628 = CARTESIAN_POINT ( 'NONE',  ( 0.000000000000000000, 87.00000000000001421, 0.000000000000000000 ) ) ;
#6629 = CYLINDRICAL_SURFACE ( 'NONE', #1217, 27.00000000000000355 ) ;
#6630 = CARTESIAN_POINT ( 'NONE',  ( -22.28244091826395135, 100.0000000000000000, -10.68852969318427881 ) ) ;
#6631 = CARTESIAN_POINT ( 'NONE',  ( 4.773458297025112707, 99.50000000000001421, -24.02094923175124208 ) ) ;
#6632 = PRODUCT_DEFINITION_FORMATION_WITH_SPECIFIED_SOURCE ( 'ANY', '', #7772, .NOT_KNOWN. ) ;
#6633 = CARTESIAN_POINT ( 'NONE',  ( -16.07368679829020763, 99.50000000000000000, 17.11560437002838952 ) ) ;
#6634 = CARTESIAN_POINT ( 'NONE',  ( 2.500000000000000000, -0.2250000000000000056, -3.061616997868383141E-16 ) ) ;
#6635 = CARTESIAN_POINT ( 'NONE',  ( 1.034219503716432668E-14, -2.812500000000000444, -2.500000000000000000 ) ) ;
#6636 = CARTESIAN_POINT ( 'NONE',  ( 3.044406660298407452, 100.0000000000000000, -23.15442635585071685 ) ) ;
#6637 = B_SPLINE_CURVE_WITH_KNOTS ( 'NONE', 1,
 ( #8430, #7756 ),
 .UNSPECIFIED., .F., .F.,
 ( 2, 2 ),
 ( 0.000000000000000000, 1.000000000000000000 ),
 .UNSPECIFIED. ) ;
#6638 = CARTESIAN_POINT ( 'NONE',  ( -19.39806930854668465, 2.349999998907525534, 19.39806930854667755 ) ) ;
#6639 = DIRECTION ( 'NONE',  ( -1.000000000000000000, 0.000000000000000000, 0.000000000000000000 ) ) ;
#6640 = CARTESIAN_POINT ( 'NONE',  ( -1.728529299398585906, -5.253648441416169490, -1.450401466387756244 ) ) ;
#6641 = VECTOR ( 'NONE', #4884, 1000.000000000000000 ) ;
#6642 = CYLINDRICAL_SURFACE ( 'NONE', #1129, 27.00000000000000355 ) ;
#6643 = LINE ( 'NONE', #6962, #2397 ) ;
#6644 = ORIENTED_EDGE ( 'NONE', *, *, #8582, .T. ) ;
#6645 =( BOUNDED_CURVE ( )  B_SPLINE_CURVE ( 2, ( #6320, #3281, #27, #6470, #7938, #1552, #3231, #4792, #8676 ),
 .UNSPECIFIED., .F., .T. ) 
 B_SPLINE_CURVE_WITH_KNOTS ( ( 3, 2, 2, 2, 3 ),
 ( 0.1041666666666666713, 0.1111111111111111049, 0.1250000000000000000, 0.1388888888888888951, 0.1458333333333333426 ),
 .UNSPECIFIED. ) 
 CURVE ( )  GEOMETRIC_REPRESENTATION_ITEM ( )  RATIONAL_B_SPLINE_CURVE ( ( 0.9330127018922194093, 0.9330127018922194093, 1.000000000000000000, 0.8660254037844387076, 1.000000000000000000, 0.8660254037844387076, 1.000000000000000000, 0.9330127018922194093, 0.9330127018922194093 ) ) 
 REPRESENTATION_ITEM ( '' )  );
#6646 = CARTESIAN_POINT ( 'NONE',  ( -21.20585021321354802, 99.50000000000005684, -9.381045134209834657 ) ) ;
#6647 = EDGE_CURVE ( 'NONE', #4141, #4703, #9069, .T. ) ;
#6648 = CARTESIAN_POINT ( 'NONE',  ( 1.679787559701184688E-15, 4.449999998907525622, -27.43301270000000258 ) ) ;
#6649 = CARTESIAN_POINT ( 'NONE',  ( 9.468852706215191262, 99.50000000000000000, 21.22967007823213237 ) ) ;
#6650 = EDGE_CURVE ( 'NONE', #1877, #600, #7475, .T. ) ;
#6651 = VECTOR ( 'NONE', #4702, 1000.000000000000000 ) ;
#6652 = CARTESIAN_POINT ( 'NONE',  ( 4.295198626299898237, 100.0000000000000142, -24.68029520312135361 ) ) ;
#6653 = CARTESIAN_POINT ( 'NONE',  ( 8.540544597724410991, 99.50000000000000000, 19.98924338346217766 ) ) ;
#6654 = CARTESIAN_POINT ( 'NONE',  ( 9.526533506306627430, 99.50000000000000000, 21.03094362668609207 ) ) ;
#6655 = CARTESIAN_POINT ( 'NONE',  ( -21.66466628782423243, 100.0000000000000142, -9.640935998098070669 ) ) ;
#6656 = VERTEX_POINT ( 'NONE', #6547 ) ;
#6657 = CARTESIAN_POINT ( 'NONE',  ( -2.500000000000000000, -4.443749998770965881, 0.000000000000000000 ) ) ;
#6658 = ORIENTED_EDGE ( 'NONE', *, *, #3520, .F. ) ;
#6659 = CARTESIAN_POINT ( 'NONE',  ( -21.43094455402013310, 100.0000000000000000, -11.42705968398779426 ) ) ;
#6660 = DIRECTION ( 'NONE',  ( -0.000000000000000000, 1.000000000000000000, -0.000000000000000000 ) ) ;
#6661 = CARTESIAN_POINT ( 'NONE',  ( -1.085030467718112069E-15, -15.00000000000000000, 3.464101615137756163 ) ) ;
#6662 = CARTESIAN_POINT ( 'NONE',  ( 4.401614252286283779, 100.0000000000000568, -24.65974366035752396 ) ) ;
#6663 = CARTESIAN_POINT ( 'NONE',  ( 8.540544597724410991, 99.50000000000000000, 19.98924338346217766 ) ) ;
#6664 = LINE ( 'NONE', #9859, #4828 ) ;
#6665 = PLANE ( 'NONE',  #797 ) ;
#6666 = CARTESIAN_POINT ( 'NONE',  ( 9.766630880609509902, 100.0000000000000284, 21.37293705761699059 ) ) ;
#6667 = DIRECTION ( 'NONE',  ( 0.000000000000000000, -1.000000000000000000, 0.000000000000000000 ) ) ;
#6668 = CARTESIAN_POINT ( 'NONE',  ( -5.039362679103552881E-15, 3.349999998907525534, 27.43301270000000258 ) ) ;
#6669 = DIRECTION ( 'NONE',  ( 0.9569724629708533659, 0.000000000000000000, -0.2901787468363226097 ) ) ;
#6670 = CARTESIAN_POINT ( 'NONE',  ( 3.434779879277784609, 99.50000000000001421, -23.17575050830969374 ) ) ;
#6671 = CARTESIAN_POINT ( 'NONE',  ( 7.726884419709978857, 99.99999999999994316, 20.74516479202295471 ) ) ;
#6672 = ORIENTED_EDGE ( 'NONE', *, *, #9277, .T. ) ;
#6673 = CARTESIAN_POINT ( 'NONE',  ( 3.403200340195960738, 99.49999999999998579, -22.39827506699316118 ) ) ;
#6674 = CARTESIAN_POINT ( 'NONE',  ( 11.18376618407357626, 5.249999997815050889, 27.00000000000000000 ) ) ;
#6675 = CYLINDRICAL_SURFACE ( 'NONE', #8446, 2.500000000000000000 ) ;
#6676 = FACE_OUTER_BOUND ( 'NONE', #4564, .T. ) ;
#6677 = EDGE_CURVE ( 'NONE', #834, #8336, #755, .T. ) ;
#6678 = CARTESIAN_POINT ( 'NONE',  ( -22.16320288552370243, 99.50000000000001421, -10.86869938533413915 ) ) ;
#6679 = DIRECTION ( 'NONE',  ( 0.000000000000000000, -1.000000000000000000, 0.000000000000000000 ) ) ;
#6680 = PLANE ( 'NONE',  #958 ) ;
#6681 = ORIENTED_EDGE ( 'NONE', *, *, #8781, .F. ) ;
#6682 = AXIS2_PLACEMENT_3D ( 'NONE', #3759, #9237, #8464 ) ;
#6683 = CARTESIAN_POINT ( 'NONE',  ( -2.499999999999999556, -0.4124999999999999778, 1.443375672974065882 ) ) ;
#6684 = CARTESIAN_POINT ( 'NONE',  ( 0.000000000000000000, -5.000000000000000000, -2.500000000000000000 ) ) ;
#6685 = CARTESIAN_POINT ( 'NONE',  ( 2.928963527206765338, 99.99999999999997158, -23.52685633767685758 ) ) ;
#6686 = CARTESIAN_POINT ( 'NONE',  ( -19.39806930854668465, 3.149999998907525356, 19.39806930854667755 ) ) ;
#6687 = CARTESIAN_POINT ( 'NONE',  ( 11.36312591709336139, 0.4999999989075251672, -27.43301270000000258 ) ) ;
#6688 = CARTESIAN_POINT ( 'NONE',  ( -20.66709314808276332, 100.0000000000000284, -10.01107456535036455 ) ) ;
#6689 = CARTESIAN_POINT ( 'NONE',  ( 0.000000000000000000, 87.00000000000001421, 0.000000000000000000 ) ) ;
#6690 = DIRECTION ( 'NONE',  ( 0.000000000000000000, 0.000000000000000000, -1.000000000000000000 ) ) ;
#6691 = EDGE_CURVE ( 'NONE', #2647, #2426, #4155, .T. ) ;
#6692 = DIRECTION ( 'NONE',  ( -0.2910078965507976179, 0.000000000000000000, -0.9567206510497618943 ) ) ;
#6693 = CYLINDRICAL_SURFACE ( 'NONE', #5635, 24.00000000000000355 ) ;
#6694 = CARTESIAN_POINT ( 'NONE',  ( 27.43301270000000258, 5.049999998907525267, 0.000000000000000000 ) ) ;
#6695 = DIRECTION ( 'NONE',  ( -0.000000000000000000, -1.000000000000000000, -0.000000000000000000 ) ) ;
#6696 = CARTESIAN_POINT ( 'NONE',  ( -4.959819536546781389E-15, 4.599999999999999645, 27.00000000000000355 ) ) ;
#6697 = DIRECTION ( 'NONE',  ( -0.000000000000000000, 1.000000000000000000, -0.000000000000000000 ) ) ;
#6698 = DIRECTION ( 'NONE',  ( -0.000000000000000000, 1.000000000000000000, -0.000000000000000000 ) ) ;
#6699 = DIRECTION ( 'NONE',  ( 0.000000000000000000, 0.000000000000000000, 1.000000000000000000 ) ) ;
#6700 = EDGE_LOOP ( 'NONE', ( #8924, #1351, #10136, #3003 ) ) ;
#6701 = EDGE_CURVE ( 'NONE', #341, #2896, #5967, .T. ) ;
#6702 =( BOUNDED_SURFACE ( )  B_SPLINE_SURFACE ( 1, 2, ( 
 ( #5018, #9781, #4190, #6687, #8214, #9880, #5119, #8317, #1149, #8478, #3718, #5400, #4442, #10042, #7688, #4496, #7798, #4662, #3875, #6900, #3771, #8592, #682, #1306, #7010, #3101, #1469, #2142, #1414, #470, #8533, #10096, #5279, #9428, #2878, #6846, #2254, #3828, #6061, #10213, #3047, #6957, #9371, #527, #9252, #2085, #629, #10160, #2935, #6227, #6117, #7745, #2200, #3666, #9310, #5343, #1358, #5455, #4550, #1252, #8645, #578, #7852, #2993, #6173, #4606, #7061, #7630, #10269, #6285, #9482, #2308, #5508, #939, #790, #841, #2460, #8110, #8745, #4081, #154, #8894, #9576, #8846, #7904, #5604, #3982, #2356, #6486, #7117, #3930, #9677, #891, #10317, #7263, #105, #4032, #3295, #5553, #48, #3201 ),
 ( #7316, #3341, #2515, #6532, #1620, #1719, #1569, #4133, #4913, #7168, #2408, #4759, #5706, #3463, #9719, #2561, #8697, #3155, #7214, #1518, #3248, #7957, #1672, #4711, #6435, #737, #6338, #9532, #6383, #8794, #4814, #8009, #9628, #5655, #4867, #8057, #1961, #1133, #5952, #5157, #9039, #9768, #1032, #7460, #6729, #2607, #5002, #8302, #200, #985, #1186, #4277, #402, #300, #4227, #9142, #8941, #3489, #3433, #9092, #8355, #1082, #4177, #7563, #3383, #7359, #1810, #8989, #1910, #4377, #3597, #8202, #8254, #9870, #6780, #5798, #4326, #9979, #5753, #6626, #5896, #4956, #2654, #7405, #248, #3540, #6577, #9819, #9925, #7510, #5844, #348, #2760, #6674, #1759, #1857, #2706, #5053, #8157, #5102, #7050 ) ),
 .UNSPECIFIED., .F., .F., .T. ) 
 B_SPLINE_SURFACE_WITH_KNOTS ( ( 2, 2 ),
 ( 3, 2, 2, 2, 2, 2, 2, 2, 2, 2, 2, 2, 2, 2, 2, 2, 2, 2, 2, 2, 2, 2, 2, 2, 2, 2, 2, 2, 2, 2, 2, 2, 2, 2, 2, 2, 2, 2, 2, 2, 2, 2, 2, 2, 2, 2, 2, 2, 2, 2, 3 ),
 ( 0.000000000000000000, 1.000000000000000000 ),
 ( 0.000000000000000000, 0.01785714285714285615, 0.03571428571428571230, 0.05357142857142856845, 0.07142857142857142461, 0.08928571428571428770, 0.1071428571428571369, 0.1250000000000000000, 0.1428571428571428492, 0.1607142857142857262, 0.1785714285714285754, 0.1964285714285714246, 0.2142857142857142738, 0.2321428571428571508, 0.2500000000000000000, 0.2678571428571428492, 0.2857142857142856984, 0.3035714285714285476, 0.3214285714285714524, 0.3392857142857143016, 0.3571428571428571508, 0.3750000000000000000, 0.3928571428571428492, 0.4107142857142856984, 0.4285714285714285476, 0.4464285714285714524, 0.4642857142857143016, 0.4821428571428571508, 0.5000000000000000000, 0.5178571428571429047, 0.5357142857142856984, 0.5535714285714286031, 0.5714285714285713969, 0.5892857142857143016, 0.6071428571428570953, 0.6250000000000000000, 0.6428571428571429047, 0.6607142857142856984, 0.6785714285714286031, 0.6964285714285713969, 0.7142857142857143016, 0.7321428571428570953, 0.7500000000000000000, 0.7678571428571429047, 0.7857142857142856984, 0.8035714285714286031, 0.8214285714285713969, 0.8392857142857143016, 0.8571428571428570953, 0.8750000000000000000, 0.8928571428571429047 ),
 .UNSPECIFIED. ) 
 GEOMETRIC_REPRESENTATION_ITEM ( )  RATIONAL_B_SPLINE_SURFACE ( (
 ( 1.000000000000000000, 0.9238795325112867385, 1.000000000000000000, 0.9238795325112867385, 1.000000000000000000, 0.9238795325112867385, 1.000000000000000000, 0.9238795325112867385, 1.000000000000000000, 0.9238795325112867385, 1.000000000000000000, 0.9238795325112867385, 1.000000000000000000, 0.9238795325112867385, 1.000000000000000000, 0.9238795325112867385, 1.000000000000000000, 0.9238795325112867385, 1.000000000000000000, 0.9238795325112867385, 1.000000000000000000, 0.9238795325112867385, 1.000000000000000000, 0.9238795325112867385, 1.000000000000000000, 0.9238795325112867385, 1.000000000000000000, 0.9238795325112867385, 1.000000000000000000, 0.9238795325112867385, 1.000000000000000000, 0.9238795325112867385, 1.000000000000000000, 0.9238795325112867385, 1.000000000000000000, 0.9238795325112867385, 1.000000000000000000, 0.9238795325112867385, 1.000000000000000000, 0.9238795325112867385, 1.000000000000000000, 0.9238795325112867385, 1.000000000000000000, 0.9238795325112867385, 1.000000000000000000, 0.9238795325112867385, 1.000000000000000000, 0.9238795325112867385, 1.000000000000000000, 0.9238795325112867385, 1.000000000000000000, 0.9238795325112867385, 1.000000000000000000, 0.9238795325112867385, 1.000000000000000000, 0.9238795325112867385, 1.000000000000000000, 0.9238795325112867385, 1.000000000000000000, 0.9238795325112867385, 1.000000000000000000, 0.9238795325112867385, 1.000000000000000000, 0.9238795325112867385, 1.000000000000000000, 0.9238795325112867385, 1.000000000000000000, 0.9238795325112867385, 1.000000000000000000, 0.9238795325112867385, 1.000000000000000000, 0.9238795325112867385, 1.000000000000000000, 0.9238795325112867385, 1.000000000000000000, 0.9238795325112867385, 1.000000000000000000, 0.9238795325112867385, 1.000000000000000000, 0.9238795325112867385, 1.000000000000000000, 0.9238795325112867385, 1.000000000000000000, 0.9238795325112867385, 1.000000000000000000, 0.9238795325112867385, 1.000000000000000000, 0.9238795325112867385, 1.000000000000000000, 0.9238795325112867385, 1.000000000000000000, 0.9238795325112867385, 1.000000000000000000, 0.9238795325112867385, 1.000000000000000000, 0.9238795325112867385, 1.000000000000000000, 0.9238795325112867385, 1.000000000000000000, 0.9238795325112867385, 1.000000000000000000),
 ( 1.000000000000000000, 0.9238795325112867385, 1.000000000000000000, 0.9238795325112867385, 1.000000000000000000, 0.9238795325112867385, 1.000000000000000000, 0.9238795325112867385, 1.000000000000000000, 0.9238795325112867385, 1.000000000000000000, 0.9238795325112867385, 1.000000000000000000, 0.9238795325112867385, 1.000000000000000000, 0.9238795325112867385, 1.000000000000000000, 0.9238795325112867385, 1.000000000000000000, 0.9238795325112867385, 1.000000000000000000, 0.9238795325112867385, 1.000000000000000000, 0.9238795325112867385, 1.000000000000000000, 0.9238795325112867385, 1.000000000000000000, 0.9238795325112867385, 1.000000000000000000, 0.9238795325112867385, 1.000000000000000000, 0.9238795325112867385, 1.000000000000000000, 0.9238795325112867385, 1.000000000000000000, 0.9238795325112867385, 1.000000000000000000, 0.9238795325112867385, 1.000000000000000000, 0.9238795325112867385, 1.000000000000000000, 0.9238795325112867385, 1.000000000000000000, 0.9238795325112867385, 1.000000000000000000, 0.9238795325112867385, 1.000000000000000000, 0.9238795325112867385, 1.000000000000000000, 0.9238795325112867385, 1.000000000000000000, 0.9238795325112867385, 1.000000000000000000, 0.9238795325112867385, 1.000000000000000000, 0.9238795325112867385, 1.000000000000000000, 0.9238795325112867385, 1.000000000000000000, 0.9238795325112867385, 1.000000000000000000, 0.9238795325112867385, 1.000000000000000000, 0.9238795325112867385, 1.000000000000000000, 0.9238795325112867385, 1.000000000000000000, 0.9238795325112867385, 1.000000000000000000, 0.9238795325112867385, 1.000000000000000000, 0.9238795325112867385, 1.000000000000000000, 0.9238795325112867385, 1.000000000000000000, 0.9238795325112867385, 1.000000000000000000, 0.9238795325112867385, 1.000000000000000000, 0.9238795325112867385, 1.000000000000000000, 0.9238795325112867385, 1.000000000000000000, 0.9238795325112867385, 1.000000000000000000, 0.9238795325112867385, 1.000000000000000000, 0.9238795325112867385, 1.000000000000000000, 0.9238795325112867385, 1.000000000000000000, 0.9238795325112867385, 1.000000000000000000, 0.9238795325112867385, 1.000000000000000000, 0.9238795325112867385, 1.000000000000000000, 0.9238795325112867385, 1.000000000000000000, 0.9238795325112867385, 1.000000000000000000) ) ) 
 REPRESENTATION_ITEM ( '' )  SURFACE ( )  );
#6703 = CARTESIAN_POINT ( 'NONE',  ( 0.000000000000000000, 99.50000000000000000, 0.000000000000000000 ) ) ;
#6704 = ADVANCED_FACE ( 'NONE', ( #1775, #316 ), #8372, .F. ) ;
#6705 = CARTESIAN_POINT ( 'NONE',  ( -2.256430356250000102, -2.053124999385482763, 0.000000000000000000 ) ) ;
#6706 = VERTEX_POINT ( 'NONE', #7476 ) ;
#6707 = CARTESIAN_POINT ( 'NONE',  ( -21.16695614262292580, 100.0000000000000000, -11.33496398805607441 ) ) ;
#6708 = CARTESIAN_POINT ( 'NONE',  ( 3.411785164761435674, 99.50000000000000000, -22.76693382491622231 ) ) ;
#6709 = EDGE_CURVE ( 'NONE', #2131, #3256, #295, .T. ) ;
#6710 = CARTESIAN_POINT ( 'NONE',  ( -11.18376618407356737, 4.849999997815050534, -27.00000000000000355 ) ) ;
#6711 = CARTESIAN_POINT ( 'NONE',  ( -15.10617644529808423, 100.0000000000000284, 15.98944417891004477 ) ) ;
#6712 = VECTOR ( 'NONE', #10008, 1000.000000000000000 ) ;
#6713 = ORIENTED_EDGE ( 'NONE', *, *, #3961, .F. ) ;
#6714 = CARTESIAN_POINT ( 'NONE',  ( -16.36254897777738648, 99.50000000000000000, 15.39785597259249172 ) ) ;
#6715 = EDGE_CURVE ( 'NONE', #6656, #4720, #3503, .T. ) ;
#6716 = CARTESIAN_POINT ( 'NONE',  ( 5.825495487346713297, 100.0000000000000000, 20.69456627699299744 ) ) ;
#6717 = DIRECTION ( 'NONE',  ( -0.1705044153832351028, 0.000000000000000000, 0.9853569121566161382 ) ) ;
#6718 = CARTESIAN_POINT ( 'NONE',  ( 3.349514647153394975, 99.49999999999998579, -23.95461210612682024 ) ) ;
#6719 = CIRCLE ( 'NONE', #8230, 27.00000000000000000 ) ;
#6720 = ORIENTED_EDGE ( 'NONE', *, *, #6350, .F. ) ;
#6721 = CARTESIAN_POINT ( 'NONE',  ( 1.653273178848927064E-15, 1.599999997815050312, -27.00000000000000355 ) ) ;
#6722 = CARTESIAN_POINT ( 'NONE',  ( 11.36312591709336139, 4.499999998907525445, -27.43301270000000258 ) ) ;
#6723 = CARTESIAN_POINT ( 'NONE',  ( -9.703070624755296135E-15, -4.837500000000001243, 2.500000000000000444 ) ) ;
#6724 = APPLICATION_CONTEXT ( 'automotive_design' ) ;
#6725 = CARTESIAN_POINT ( 'NONE',  ( 3.635130212803377781, 99.99999999999997158, -23.00575896550913768 ) ) ;
#6726 = CARTESIAN_POINT ( 'NONE',  ( 7.809833820264425519, 99.99999999999991473, 20.29999375863051370 ) ) ;
#6727 = EDGE_LOOP ( 'NONE', ( #434, #5134 ) ) ;
#6728 = CARTESIAN_POINT ( 'NONE',  ( 3.411785164761435674, 99.50000000000000000, -22.76693382491622231 ) ) ;
#6729 = CARTESIAN_POINT ( 'NONE',  ( -4.959819536546781389E-15, 2.799999997815050268, 27.00000000000000355 ) ) ;
#6730 = COLOUR_RGB ( '',0.8941176470588234615, 0.8941176470588234615, 0.8941176470588234615 ) ;
#6731 = CARTESIAN_POINT ( 'NONE',  ( 0.000000000000000000, 0.000000000000000000, 0.000000000000000000 ) ) ;
#6732 = CARTESIAN_POINT ( 'NONE',  ( -2.499999999999999112, -0.4124999999999999223, 1.443375672974065882 ) ) ;
#6733 = CARTESIAN_POINT ( 'NONE',  ( 0.000000000000000000, 0.000000000000000000, 0.000000000000000000 ) ) ;
#6734 = CARTESIAN_POINT ( 'NONE',  ( 0.000000000000000000, 0.000000000000000000, -2.500000000000000000 ) ) ;
#6735 = CARTESIAN_POINT ( 'NONE',  ( -2.500000000000000000, -2.287499999999999645, -1.443375672974064106 ) ) ;
#6736 = VERTEX_POINT ( 'NONE', #215 ) ;
#6737 = CARTESIAN_POINT ( 'NONE',  ( -1.249999999999998224, -1.724999999999999645, 2.165063509461097713 ) ) ;
#6738 = EDGE_CURVE ( 'NONE', #3772, #4679, #8171, .T. ) ;
#6739 = DIRECTION ( 'NONE',  ( 1.000000000000000000, 0.000000000000000000, 0.000000000000000000 ) ) ;
#6740 = CARTESIAN_POINT ( 'NONE',  ( -14.79004890936967875, 99.49999999999998579, 16.19006955939758541 ) ) ;
#6741 = DIRECTION ( 'NONE',  ( 0.000000000000000000, 1.000000000000000000, -0.000000000000000000 ) ) ;
#6742 = CARTESIAN_POINT ( 'NONE',  ( 27.43301270000000258, 2.699999998907525178, -11.36312591709336139 ) ) ;
#6743 = CARTESIAN_POINT ( 'NONE',  ( -1.250000000000000222, -0.9749999999999999778, -2.165063509461096825 ) ) ;
#6744 = ORIENTED_EDGE ( 'NONE', *, *, #4960, .T. ) ;
#6745 = CARTESIAN_POINT ( 'NONE',  ( 3.411785164761435674, 99.50000000000000000, -22.76693382491622231 ) ) ;
#6746 = DIRECTION ( 'NONE',  ( -0.000000000000000000, 1.000000000000000000, -0.000000000000000000 ) ) ;
#6747 = SURFACE_SIDE_STYLE ('',( #5174 ) ) ;
#6748 = DIRECTION ( 'NONE',  ( 0.000000000000000000, -1.000000000000000000, 0.000000000000000000 ) ) ;
#6749 = LINE ( 'NONE', #4400, #8290 ) ;
#6750 = CARTESIAN_POINT ( 'NONE',  ( -1.128215178124998497, -0.5156249993854828961, 1.954126010382872147 ) ) ;
#6751 = CARTESIAN_POINT ( 'NONE',  ( -11.36312591709335962, 0.4999999989075251672, -27.43301270000000258 ) ) ;
#6752 =( NAMED_UNIT ( * ) PLANE_ANGLE_UNIT ( ) SI_UNIT ( $, .RADIAN. ) );
#6753 = CARTESIAN_POINT ( 'NONE',  ( 9.877377282685029372E-16, -0.7874999999999998668, 2.500000000000000000 ) ) ;
#6754 = EDGE_CURVE ( 'NONE', #3778, #5950, #5500, .T. ) ;
#6755 = CARTESIAN_POINT ( 'NONE',  ( 0.000000000000000000, 0.000000000000000000, 0.000000000000000000 ) ) ;
#6756 = DIRECTION ( 'NONE',  ( -0.000000000000000000, 1.000000000000000000, -0.000000000000000000 ) ) ;
#6757 = VERTEX_POINT ( 'NONE', #2722 ) ;
#6758 = CARTESIAN_POINT ( 'NONE',  ( -16.30427144417478402, 99.99999999999998579, 16.48895498912494517 ) ) ;
#6759 = CARTESIAN_POINT ( 'NONE',  ( 2.256430356250000102, -1.828124999385482674, -2.763330213280484622E-16 ) ) ;
#6760 = ORIENTED_EDGE ( 'NONE', *, *, #512, .F. ) ;
#6761 = CARTESIAN_POINT ( 'NONE',  ( 7.156925775808251622, 100.0000000000000000, 23.91622092442889524 ) ) ;
#6762 = CARTESIAN_POINT ( 'NONE',  ( 27.43301270000000258, 0.2499999989075252504, 0.000000000000000000 ) ) ;
#6763 = CIRCLE ( 'NONE', #8947, 27.00000000000000355 ) ;
#6764 = DIRECTION ( 'NONE',  ( -0.000000000000000000, 1.000000000000000000, -0.000000000000000000 ) ) ;
#6765 = CARTESIAN_POINT ( 'NONE',  ( -15.32348647777738826, 100.0000000000000000, 15.39505148541300450 ) ) ;
#6766 =( BOUNDED_CURVE ( )  B_SPLINE_CURVE ( 2, ( #7060, #4605, #628, #2934, #7797 ),
 .UNSPECIFIED., .F., .F. ) 
 B_SPLINE_CURVE_WITH_KNOTS ( ( 3, 2, 3 ),
 ( 0.000000000000000000, 0.01785714285714285615, 0.03571428571428571230 ),
 .UNSPECIFIED. ) 
 CURVE ( )  GEOMETRIC_REPRESENTATION_ITEM ( )  RATIONAL_B_SPLINE_CURVE ( ( 1.000000000000000000, 0.9238795325112867385, 1.000000000000000000, 0.9238795325112867385, 1.000000000000000000 ) ) 
 REPRESENTATION_ITEM ( '' )  );
#6767 = VERTEX_POINT ( 'NONE', #6593 ) ;
#6768 = CARTESIAN_POINT ( 'NONE',  ( -11.18376618407358336, 2.949999999999999289, 26.99999999999999645 ) ) ;
#6769 = FACE_OUTER_BOUND ( 'NONE', #3189, .T. ) ;
#6770 = ORIENTED_EDGE ( 'NONE', *, *, #310, .T. ) ;
#6771 = CARTESIAN_POINT ( 'NONE',  ( 9.915951879163557692, 100.0000000000000284, 20.63215000232408158 ) ) ;
#6772 = ORIENTED_EDGE ( 'NONE', *, *, #10299, .T. ) ;
#6773 = ADVANCED_FACE ( 'NONE', ( #2777 ), #9885, .T. ) ;
#6774 = CARTESIAN_POINT ( 'NONE',  ( 21.79306891025641235, 100.0000000000000000, -1.065004006410256387 ) ) ;
#6775 = CARTESIAN_POINT ( 'NONE',  ( -11.36312591709335962, 4.599999998907525978, -27.43301270000000258 ) ) ;
#6776 = ADVANCED_FACE ( 'NONE', ( #9105 ), #6642, .T. ) ;
#6777 = DIRECTION ( 'NONE',  ( -0.000000000000000000, 1.000000000000000000, -0.000000000000000000 ) ) ;
#6778 = ORIENTED_EDGE ( 'NONE', *, *, #3277, .F. ) ;
#6779 = CARTESIAN_POINT ( 'NONE',  ( 5.825495487346713297, 99.50000000000000000, 20.69456627699299744 ) ) ;
#6780 = CARTESIAN_POINT ( 'NONE',  ( -19.09188309203678813, 4.299999997815050712, 19.09188309203678457 ) ) ;
#6781 = CARTESIAN_POINT ( 'NONE',  ( -22.57971655928959365, 99.50000000000000000, -10.84768434062017839 ) ) ;
#6782 = FACE_BOUND ( 'NONE', #336, .T. ) ;
#6783 = CARTESIAN_POINT ( 'NONE',  ( 0.000000000000000000, 85.00000000000000000, 0.000000000000000000 ) ) ;
#6784 = ORIENTED_EDGE ( 'NONE', *, *, #42, .T. ) ;
#6785 = CARTESIAN_POINT ( 'NONE',  ( 4.803433990161294354, 100.0000000000000142, -23.96838578116891583 ) ) ;
#6786 = CARTESIAN_POINT ( 'NONE',  ( -19.39806930854667755, 2.249999998907525001, -19.39806930854668110 ) ) ;
#6787 = ORIENTED_EDGE ( 'NONE', *, *, #9948, .F. ) ;
#6788 = VECTOR ( 'NONE', #609, 1000.000000000000114 ) ;
#6789 = CARTESIAN_POINT ( 'NONE',  ( 2.500000000000000444, -0.7124999999999999112, 1.443375672974063439 ) ) ;
#6790 = DIRECTION ( 'NONE',  ( 0.000000000000000000, 1.000000000000000000, 0.000000000000000000 ) ) ;
#6791 = DIRECTION ( 'NONE',  ( 0.000000000000000000, -0.000000000000000000, 1.000000000000000000 ) ) ;
#6792 = CARTESIAN_POINT ( 'NONE',  ( 1.128215178125001161, -1.903124999385482852, 1.954126010382870815 ) ) ;
#6793 = CARTESIAN_POINT ( 'NONE',  ( 19.39806930854667399, 3.349999998907525534, 19.39806930854668465 ) ) ;
#6794 = CARTESIAN_POINT ( 'NONE',  ( 1.249999999999999334, -0.5437499987709658589, -2.165063509461096825 ) ) ;
#6795 = ORIENTED_EDGE ( 'NONE', *, *, #4869, .F. ) ;
#6796 = CARTESIAN_POINT ( 'NONE',  ( 9.600410285814406919, 99.99999999999998579, 19.87914582625927196 ) ) ;
#6797 = CARTESIAN_POINT ( 'NONE',  ( 4.386516977709190357, 100.0000000000000426, -24.31220192127581825 ) ) ;
#6798 =( LENGTH_UNIT ( ) NAMED_UNIT ( * ) SI_UNIT ( .MILLI., .METRE. ) );
#6799 = CARTESIAN_POINT ( 'NONE',  ( 4.054941747578200584, 99.99999999999998579, -24.36678493958047298 ) ) ;
#6800 = CARTESIAN_POINT ( 'NONE',  ( 5.725936192474917696, 99.50000000000000000, 21.08018326417248645 ) ) ;
#6801 = CARTESIAN_POINT ( 'NONE',  ( -21.16695614262292580, 99.50000000000000000, -11.33496398805607441 ) ) ;
#6802 = VERTEX_POINT ( 'NONE', #7581 ) ;
#6803 = DIRECTION ( 'NONE',  ( 0.000000000000000000, 1.000000000000000000, 0.000000000000000000 ) ) ;
#6804 = CARTESIAN_POINT ( 'NONE',  ( -27.43301270000000258, 1.449999998907525178, -3.359575119402369376E-15 ) ) ;
#6805 =( NAMED_UNIT ( * ) SI_UNIT ( $, .STERADIAN. ) SOLID_ANGLE_UNIT ( ) );
#6806 = CARTESIAN_POINT ( 'NONE',  ( 4.128176300878408256, 100.0000000000000142, -21.47174600747824869 ) ) ;
#6807 = CARTESIAN_POINT ( 'NONE',  ( 3.222930479149370253, 99.49999999999995737, -22.15251218086615381 ) ) ;
#6808 = CARTESIAN_POINT ( 'NONE',  ( -15.07178375341841381, 99.50000000000000000, 16.66969090848992607 ) ) ;
#6809 = EDGE_LOOP ( 'NONE', ( #7912, #2636, #8092, #1928 ) ) ;
#6810 = VERTEX_POINT ( 'NONE', #1151 ) ;
#6811 = DIRECTION ( 'NONE',  ( 0.000000000000000000, 0.000000000000000000, -1.000000000000000000 ) ) ;
#6812 = CARTESIAN_POINT ( 'NONE',  ( -1.128215178124998497, -2.428124999385482763, 1.954126010382872147 ) ) ;
#6813 = VERTEX_POINT ( 'NONE', #1825 ) ;
#6814 = ADVANCED_FACE ( 'NONE', ( #8270 ), #3454, .T. ) ;
#6815 = VECTOR ( 'NONE', #2668, 1000.000000000000000 ) ;
#6816 = DIRECTION ( 'NONE',  ( 0.000000000000000000, 0.000000000000000000, -1.000000000000000000 ) ) ;
#6817 = CARTESIAN_POINT ( 'NONE',  ( -11.36312591709335962, 0.4999999989075252782, -27.43301270000000258 ) ) ;
#6818 = CARTESIAN_POINT ( 'NONE',  ( -19.46743691185369585, 99.50000000000000000, -8.912588186774021537 ) ) ;
#6819 = CARTESIAN_POINT ( 'NONE',  ( 4.401614252286283779, 99.50000000000002842, -24.65974366035752396 ) ) ;
#6820 = DIRECTION ( 'NONE',  ( -0.000000000000000000, -1.000000000000000000, -0.000000000000000000 ) ) ;
#6821 = CARTESIAN_POINT ( 'NONE',  ( -16.91659681606879317, 100.0000000000000000, 15.78485274883190392 ) ) ;
#6822 = CARTESIAN_POINT ( 'NONE',  ( -4.959819536546781389E-15, 0.6000000000000000888, 27.00000000000000355 ) ) ;
#6823 = ORIENTED_EDGE ( 'NONE', *, *, #9480, .T. ) ;
#6824 = CARTESIAN_POINT ( 'NONE',  ( -10.49999999999999822, 104.5000000000000142, 0.000000000000000000 ) ) ;
#6825 = CARTESIAN_POINT ( 'NONE',  ( 1.679787559701184688E-15, 3.749999998907525445, -27.43301270000000258 ) ) ;
#6826 = DIRECTION ( 'NONE',  ( 1.000000000000000000, 0.000000000000000000, 0.000000000000000000 ) ) ;
#6827 = CARTESIAN_POINT ( 'NONE',  ( -2.781278341185190239, -20.00000000000000000, -1.353213781785880476 ) ) ;
#6828 = ORIENTED_EDGE ( 'NONE', *, *, #2801, .F. ) ;
#6829 = CARTESIAN_POINT ( 'NONE',  ( -1.249999999999998224, -0.7687499987709658367, 2.165063509461097713 ) ) ;
#6830 = PRODUCT_RELATED_PRODUCT_CATEGORY ( 'part', '', ( #1333 ) ) ;
#6831 = DIRECTION ( 'NONE',  ( 0.000000000000000000, 1.000000000000000000, 0.000000000000000000 ) ) ;
#6832 = EDGE_CURVE ( 'NONE', #3838, #9728, #418, .T. ) ;
#6833 = DIRECTION ( 'NONE',  ( 0.000000000000000000, 1.000000000000000000, 0.000000000000000000 ) ) ;
#6834 = DIRECTION ( 'NONE',  ( 0.000000000000000000, -1.000000000000000000, 0.000000000000000000 ) ) ;
#6835 = CARTESIAN_POINT ( 'NONE',  ( 3.504547665631520648, 99.99999999999997158, -23.10026541809159184 ) ) ;
#6836 = EDGE_CURVE ( 'NONE', #7711, #2107, #7235, .T. ) ;
#6837 = ORIENTED_EDGE ( 'NONE', *, *, #7813, .T. ) ;
#6838 = CARTESIAN_POINT ( 'NONE',  ( -16.61132721736409934, 100.0000000000000142, 16.61681399495993716 ) ) ;
#6839 = CARTESIAN_POINT ( 'NONE',  ( 19.39806930854668110, 2.049999998907525711, -19.39806930854668110 ) ) ;
#6840 = ORIENTED_EDGE ( 'NONE', *, *, #1716, .F. ) ;
#6841 = CARTESIAN_POINT ( 'NONE',  ( -1.249999999999998224, -0.8249999999999998446, 2.165063509461097713 ) ) ;
#6842 = DIRECTION ( 'NONE',  ( 0.000000000000000000, 0.000000000000000000, 1.000000000000000000 ) ) ;
#6843 = CARTESIAN_POINT ( 'NONE',  ( 0.000000000000000000, -20.00000000000000000, -2.500000000000000444 ) ) ;
#6844 = CARTESIAN_POINT ( 'NONE',  ( -1.595409442497313560E-16, -1.265624999385482896, -2.605501347177161087 ) ) ;
#6845 = DIRECTION ( 'NONE',  ( -0.000000000000000000, -1.000000000000000000, -0.000000000000000000 ) ) ;
#6846 = CARTESIAN_POINT ( 'NONE',  ( 11.36312591709336139, 2.099999998907525089, -27.43301270000000258 ) ) ;
#6847 = ORIENTED_EDGE ( 'NONE', *, *, #500, .F. ) ;
#6848 = CARTESIAN_POINT ( 'NONE',  ( -16.38049141020750099, 100.0000000000000426, 14.97568473612765416 ) ) ;
#6849 = DIRECTION ( 'NONE',  ( 0.000000000000000000, -1.000000000000000000, 0.000000000000000000 ) ) ;
#6850 = DIRECTION ( 'NONE',  ( 0.000000000000000000, 0.000000000000000000, 1.000000000000000000 ) ) ;
#6851 = CARTESIAN_POINT ( 'NONE',  ( -15.91768310440539658, 100.0000000000000284, 15.18344740530786652 ) ) ;
#6852 = AXIS2_PLACEMENT_3D ( 'NONE', #8990, #6627, #4327 ) ;
#6853 = CARTESIAN_POINT ( 'NONE',  ( 4.786228327491940187E-16, -1.828124999385482674, 2.605501347177161087 ) ) ;
#6854 = PLANE ( 'NONE',  #2456 ) ;
#6855 = ORIENTED_EDGE ( 'NONE', *, *, #7681, .F. ) ;
#6856 = CARTESIAN_POINT ( 'NONE',  ( 0.000000000000000000, 97.50000000000000000, 0.000000000000000000 ) ) ;
#6857 = CARTESIAN_POINT ( 'NONE',  ( -27.43301270000000969, 1.499999998907525223, 11.36312591709335429 ) ) ;
#6858 = FILL_AREA_STYLE_COLOUR ( '', #5422 ) ;
#6859 = ORIENTED_EDGE ( 'NONE', *, *, #9357, .T. ) ;
#6860 = CARTESIAN_POINT ( 'NONE',  ( -15.29853103387017121, 99.99999999999997158, 14.98378122532347057 ) ) ;
#6861 = CARTESIAN_POINT ( 'NONE',  ( 9.554054106072296548, 99.99999999999994316, 20.45778517829714360 ) ) ;
#6862 = CYLINDRICAL_SURFACE ( 'NONE', #4119, 27.00000000000000355 ) ;
#6863 = VERTEX_POINT ( 'NONE', #7525 ) ;
#6864 = ORIENTED_EDGE ( 'NONE', *, *, #3903, .T. ) ;
#6865 = CARTESIAN_POINT ( 'NONE',  ( -16.11976138926855739, 99.49999999999997158, 16.60078749809536447 ) ) ;
#6866 = B_SPLINE_CURVE_WITH_KNOTS ( 'NONE', 3,
 ( #432, #3573, #7594, #5922, #9217, #4514, #7709, #8440, #544, #9170, #2898 ),
 .UNSPECIFIED., .F., .F.,
 ( 4, 1, 1, 1, 1, 1, 1, 1, 4 ),
 ( 0.000000000000000000, 0.1514666391271576040, 0.2940212016997327260, 0.4289076436562640482, 0.5568069201790899481, 0.6759213874835566793, 0.7888117551744765477, 0.8972989960681465593, 1.000000000000000000 ),
 .UNSPECIFIED. ) ;
#6867 = CARTESIAN_POINT ( 'NONE',  ( -1.595409442497313560E-16, -1.715624999385482630, -2.605501347177161087 ) ) ;
#6868 = ORIENTED_EDGE ( 'NONE', *, *, #2074, .T. ) ;
#6869 = CARTESIAN_POINT ( 'NONE',  ( -22.31427554260534052, 99.50000000000002842, -10.13077409178744404 ) ) ;
#6870 = CARTESIAN_POINT ( 'NONE',  ( -15.58193289918752278, 100.0000000000000000, 16.98546238400348329 ) ) ;
#6871 = CARTESIAN_POINT ( 'NONE',  ( 3.306546357697854128E-15, 100.0000000000000000, 27.00000000000000355 ) ) ;
#6872 = CARTESIAN_POINT ( 'NONE',  ( -1.128215178124998497, -1.978124999385482807, 1.954126010382872147 ) ) ;
#6873 = CARTESIAN_POINT ( 'NONE',  ( 3.044406660298407452, 100.0000000000000000, -23.15442635585071685 ) ) ;
#6874 = EDGE_CURVE ( 'NONE', #3644, #6902, #367, .T. ) ;
#6875 = VECTOR ( 'NONE', #10013, 1000.000000000000000 ) ;
#6876 = VECTOR ( 'NONE', #3611, 1000.000000000000000 ) ;
#6877 = LINE ( 'NONE', #7663, #5821 ) ;
#6878 = LINE ( 'NONE', #1394, #6788 ) ;
#6879 = EDGE_LOOP ( 'NONE', ( #1376, #9472 ) ) ;
#6880 = LINE ( 'NONE', #6824, #4572 ) ;
#6881 = CARTESIAN_POINT ( 'NONE',  ( 11.36312591709336850, 4.199999998907525622, 27.43301269999999903 ) ) ;
#6882 = CARTESIAN_POINT ( 'NONE',  ( 2.256430356249999658, -0.7781249993854829627, -1.302750673588581432 ) ) ;
#6883 = CARTESIAN_POINT ( 'NONE',  ( 9.915951879163557692, 100.0000000000000142, 20.63215000232408158 ) ) ;
#6884 = ADVANCED_FACE ( 'NONE', ( #3774 ), #5226, .F. ) ;
#6885 = ORIENTED_EDGE ( 'NONE', *, *, #4220, .F. ) ;
#6886 = CARTESIAN_POINT ( 'NONE',  ( -21.03505001771060634, 100.0000000000000000, -9.476849197711761263 ) ) ;
#6887 = CARTESIAN_POINT ( 'NONE',  ( 4.599186066243659887, 99.50000000000002842, -24.59301055568561623 ) ) ;
#6888 = DIRECTION ( 'NONE',  ( -0.000000000000000000, 1.000000000000000000, -0.000000000000000000 ) ) ;
#6889 = CARTESIAN_POINT ( 'NONE',  ( -4.959819536546781389E-15, 5.199999997815050179, 27.00000000000000355 ) ) ;
#6890 = ORIENTED_EDGE ( 'NONE', *, *, #6701, .F. ) ;
#6891 = CARTESIAN_POINT ( 'NONE',  ( -15.43596444985078975, 100.0000000000000284, 15.30036492734783593 ) ) ;
#6892 = CARTESIAN_POINT ( 'NONE',  ( 27.43301270000000258, 1.999999998907525001, -11.36312591709336139 ) ) ;
#6893 = ORIENTED_EDGE ( 'NONE', *, *, #5943, .F. ) ;
#6894 = CARTESIAN_POINT ( 'NONE',  ( 2.500000000000000000, -0.6374999999999999556, -1.443375672974064994 ) ) ;
#6895 = SHAPE_DEFINITION_REPRESENTATION ( #1421, #177 ) ;
#6896 = CARTESIAN_POINT ( 'NONE',  ( 2.500000000000000000, -2.381249998770965437, -1.443375672974065438 ) ) ;
#6897 = CARTESIAN_POINT ( 'NONE',  ( 2.955068081869620666, 99.99999999999995737, -21.57801138750623338 ) ) ;
#6898 = CARTESIAN_POINT ( 'NONE',  ( 1.128215178124999607, -2.653124999385482408, -1.954126010382871259 ) ) ;
#6899 = CARTESIAN_POINT ( 'NONE',  ( -27.43301270000000258, 4.649999998907525800, -3.359575119402369376E-15 ) ) ;
#6900 = CARTESIAN_POINT ( 'NONE',  ( 11.36312591709336139, 1.299999998907525267, -27.43301270000000258 ) ) ;
#6901 = AXIS2_PLACEMENT_3D ( 'NONE', #2122, #8400, #1955 ) ;
#6903 = EDGE_LOOP ( 'NONE', ( #2255, #2470, #6561, #2151 ) ) ;
#6902 = VERTEX_POINT ( 'NONE', #2088 ) ;
#6904 = CARTESIAN_POINT ( 'NONE',  ( 2.500000000000000000, -1.987499999999999600, -1.443375672974065438 ) ) ;
#6905 = CARTESIAN_POINT ( 'NONE',  ( 4.232798786556307036, 100.0000000000000000, -24.34936571594186105 ) ) ;
#6906 = CARTESIAN_POINT ( 'NONE',  ( -16.49816537377288128, 99.50000000000000000, 16.70951083495554101 ) ) ;
#6907 = CARTESIAN_POINT ( 'NONE',  ( 0.000000000000000000, 0.000000000000000000, 0.000000000000000000 ) ) ;
#6908 = ORIENTED_EDGE ( 'NONE', *, *, #7239, .T. ) ;
#6909 = CARTESIAN_POINT ( 'NONE',  ( -1.595409442497313560E-16, -0.7031249993854830072, -2.605501347177161087 ) ) ;
#6910 = CARTESIAN_POINT ( 'NONE',  ( 2.964854786877021642, 100.0000000000000000, -22.43901021186594846 ) ) ;
#6911 = EDGE_LOOP ( 'NONE', ( #6023, #9540 ) ) ;
#6912 = CARTESIAN_POINT ( 'NONE',  ( -0.6698729810778054627, -1.201346188203299858, 2.500000000000000000 ) ) ;
#6913 = CARTESIAN_POINT ( 'NONE',  ( 1.679787559701184688E-15, 3.649999998907525356, -27.43301270000000258 ) ) ;
#6914 = CARTESIAN_POINT ( 'NONE',  ( 1.034219503716432668E-14, -3.262500000000000178, -2.500000000000000000 ) ) ;
#6915 = EDGE_CURVE ( 'NONE', #8764, #9182, #8494, .T. ) ;
#6916 = CARTESIAN_POINT ( 'NONE',  ( 0.000000000000000000, 100.0000000000000000, -27.00000000000000355 ) ) ;
#6917 = CARTESIAN_POINT ( 'NONE',  ( 8.564701892180647036, 100.0000000000000284, 19.97971282122689018 ) ) ;
#6918 = EDGE_LOOP ( 'NONE', ( #5492, #5009, #8294, #6644 ) ) ;
#6919 = ORIENTED_EDGE ( 'NONE', *, *, #9527, .T. ) ;
#6920 = DIRECTION ( 'NONE',  ( -0.000000000000000000, -1.000000000000000000, -0.000000000000000000 ) ) ;
#6921 = CARTESIAN_POINT ( 'NONE',  ( -2.256430356250000102, -1.190624999385482941, -1.302750673588580321 ) ) ;
#6922 = VERTEX_POINT ( 'NONE', #9997 ) ;
#6923 = CARTESIAN_POINT ( 'NONE',  ( 3.306546357697853733E-15, 5.000000000000000000, 27.00000000000000000 ) ) ;
#6924 = CARTESIAN_POINT ( 'NONE',  ( 1.679787559701184688E-15, 0.4499999989075252338, -27.43301270000000258 ) ) ;
#6925 = CARTESIAN_POINT ( 'NONE',  ( -21.87421819196487505, 99.50000000000000000, -9.684578881761979119 ) ) ;
#6926 = B_SPLINE_SURFACE_WITH_KNOTS ( 'NONE', 3, 1, ( 
 ( #4407, #7590 ),
 ( #9953, #9896 ),
 ( #9116, #4300 ),
 ( #375, #1883 ),
 ( #4457, #8226 ),
 ( #1935, #1267 ),
 ( #6654, #1161 ),
 ( #1987, #5077 ),
 ( #3678, #5185 ),
 ( #3466, #7647 ),
 ( #1833, #9067 ),
 ( #5029, #484 ),
 ( #7486, #6861 ),
 ( #10058, #5132 ),
 ( #1059, #8384 ) ),
 .UNSPECIFIED., .F., .F., .F.,
 ( 4, 1, 1, 1, 1, 1, 1, 1, 1, 1, 1, 1, 4 ),
 ( 2, 2 ),
 ( 0.000000000000000000, 0.1101401978779246588, 0.2116695470404897084, 0.3047824012491699430, 0.3893374185178356539, 0.4648567744508144695, 0.5325800579573772842, 0.5913915682020929321, 0.6424829260185016544, 0.7344861914544180692, 0.8232371011010507500, 0.9113455750355911045, 1.000000000000000000 ),
 ( 0.000000000000000000, 1.000000000000000000 ),
 .UNSPECIFIED. ) ;
#6927 = CARTESIAN_POINT ( 'NONE',  ( 2.256430356250000102, -1.828124999385482674, -2.763330213280484622E-16 ) ) ;
#6928 =( BOUNDED_CURVE ( )  B_SPLINE_CURVE ( 2, ( #5266, #4484, #6048, #6104, #8408, #9926, #617, #457, #1239 ),
 .UNSPECIFIED., .F., .F. ) 
 B_SPLINE_CURVE_WITH_KNOTS ( ( 3, 2, 2, 2, 3 ),
 ( 0.6458333333333333703, 0.6527777777777777901, 0.6666666666666666297, 0.6805555555555555802, 0.6875000000000000000 ),
 .UNSPECIFIED. ) 
 CURVE ( )  GEOMETRIC_REPRESENTATION_ITEM ( )  RATIONAL_B_SPLINE_CURVE ( ( 0.9330127018922192983, 0.9330127018922198534, 1.000000000000000000, 0.8660254037844387076, 1.000000000000000000, 0.8660254037844387076, 1.000000000000000000, 0.9330127018922194093, 0.9330127018922194093 ) ) 
 REPRESENTATION_ITEM ( '' )  );
#6929 = LINE ( 'NONE', #6986, #3221 ) ;
#6930 = CARTESIAN_POINT ( 'NONE',  ( 19.09188309203678813, 4.699999997815051067, -19.09188309203678813 ) ) ;
#6931 = B_SPLINE_CURVE_WITH_KNOTS ( 'NONE', 3,
 ( #665, #1554, #3859, #5540, #10252, #8731, #3083, #6267, #9464, #2292, #2546, #6421, #1658, #4991, #3370, #8042, #4849, #4210, #8880 ),
 .UNSPECIFIED., .F., .F.,
 ( 4, 1, 1, 1, 1, 1, 1, 1, 1, 1, 1, 1, 1, 1, 1, 1, 4 ),
 ( 0.000000000000000000, 0.07024023345195122559, 0.1375772235014411093, 0.2026681864156774648, 0.2655894380381068620, 0.3279415367477454546, 0.3896445486312665740, 0.4521557380645868096, 0.5154465764363311830, 0.5785479733725392704, 0.6397241484143471046, 0.6996998702489094502, 0.7590513234224176564, 0.8180896689983322423, 0.8773873076253557723, 0.9378402036119877216, 1.000000000000000000 ),
 .UNSPECIFIED. ) ;
#6932 = CARTESIAN_POINT ( 'NONE',  ( 1.249999999999999334, -0.9937499987709658145, -2.165063509461096825 ) ) ;
#6933 = VECTOR ( 'NONE', #9370, 1000.000000000000000 ) ;
#6934 = CARTESIAN_POINT ( 'NONE',  ( 0.000000000000000000, 0.000000000000000000, 0.000000000000000000 ) ) ;
#6935 = CARTESIAN_POINT ( 'NONE',  ( 9.554054106072296548, 100.0000000000000142, 20.45778517829714360 ) ) ;
#6936 = LINE ( 'NONE', #6154, #9742 ) ;
#6937 = CARTESIAN_POINT ( 'NONE',  ( 9.877377282685029372E-16, -4.387499999999999289, 2.500000000000000000 ) ) ;
#6938 = CARTESIAN_POINT ( 'NONE',  ( -2.256430356250000102, -2.428124999385482319, -1.302750673588580321 ) ) ;
#6939 = CARTESIAN_POINT ( 'NONE',  ( 3.061616997868383141E-16, 0.000000000000000000, 2.500000000000000000 ) ) ;
#6940 = VECTOR ( 'NONE', #6477, 1000.000000000000000 ) ;
#6941 = EDGE_LOOP ( 'NONE', ( #7678, #9241, #4151, #5011 ) ) ;
#6942 = FACE_OUTER_BOUND ( 'NONE', #198, .T. ) ;
#6943 = DIRECTION ( 'NONE',  ( 0.000000000000000000, -0.000000000000000000, -1.000000000000000000 ) ) ;
#6944 = DIRECTION ( 'NONE',  ( -0.000000000000000000, 1.000000000000000000, -0.000000000000000000 ) ) ;
#6945 = VECTOR ( 'NONE', #3804, 1000.000000000000114 ) ;
#6946 = CARTESIAN_POINT ( 'NONE',  ( 0.000000000000000000, 87.00000000000001421, 0.000000000000000000 ) ) ;
#6947 = ORIENTED_EDGE ( 'NONE', *, *, #7743, .F. ) ;
#6948 = DIRECTION ( 'NONE',  ( -1.224646799147353207E-16, 0.000000000000000000, -1.000000000000000000 ) ) ;
#6949 = LINE ( 'NONE', #7791, #4289 ) ;
#6950 = EDGE_LOOP ( 'NONE', ( #2234, #3067, #3847, #9197 ) ) ;
#6951 = EDGE_CURVE ( 'NONE', #1438, #3772, #7751, .T. ) ;
#6952 = CARTESIAN_POINT ( 'NONE',  ( -2.499999999999999556, -4.912499999999998757, 1.443375672974065882 ) ) ;
#6953 = DIRECTION ( 'NONE',  ( 1.000000000000000000, 0.000000000000000000, 0.000000000000000000 ) ) ;
#6954 = DIRECTION ( 'NONE',  ( -0.000000000000000000, 1.000000000000000000, -0.000000000000000000 ) ) ;
#6955 = CARTESIAN_POINT ( 'NONE',  ( -2.256430356250000102, -1.153124999385482852, 0.000000000000000000 ) ) ;
#6956 = CARTESIAN_POINT ( 'NONE',  ( -20.95611194834973645, 99.50000000000000000, -10.07788454426966318 ) ) ;
#6957 = CARTESIAN_POINT ( 'NONE',  ( -27.43301270000000969, 2.399999998907525356, 11.36312591709335429 ) ) ;
#6958 = ORIENTED_EDGE ( 'NONE', *, *, #4115, .T. ) ;
#6959 = UNCERTAINTY_MEASURE_WITH_UNIT (LENGTH_MEASURE( 1.000000000000000082E-05 ), #9686, 'distance_accuracy_value', 'NONE');
#6960 = CARTESIAN_POINT ( 'NONE',  ( -15.31787750341841559, 100.0000000000000000, 16.43551622900274722 ) ) ;
#6961 = CARTESIAN_POINT ( 'NONE',  ( -0.6698729810778020211, -3.186153809338631238, -2.500000000000002665 ) ) ;
#6962 = CARTESIAN_POINT ( 'NONE',  ( -2.449293598294706513E-15, 85.00000000000000000, 20.00000000000000000 ) ) ;
#6963 = CARTESIAN_POINT ( 'NONE',  ( 3.888553205800344248, 99.99999999999995737, -24.35333287445124739 ) ) ;
#6964 = VECTOR ( 'NONE', #2097, 1000.000000000000000 ) ;
#6965 = ORIENTED_EDGE ( 'NONE', *, *, #7604, .F. ) ;
#6966 = CARTESIAN_POINT ( 'NONE',  ( 2.256430356250000102, -0.8156249993854829405, -2.763330213280484622E-16 ) ) ;
#6967 = CARTESIAN_POINT ( 'NONE',  ( 3.681717055787076642, 100.0000000000000000, -21.09125273517263111 ) ) ;
#6968 = ORIENTED_EDGE ( 'NONE', *, *, #1731, .F. ) ;
#6969 = FACE_OUTER_BOUND ( 'NONE', #7071, .T. ) ;
#6970 = CARTESIAN_POINT ( 'NONE',  ( 11.36312591709336850, 2.499999998907525445, 27.43301269999999903 ) ) ;
#6971 = CIRCLE ( 'NONE', #6318, 18.23673019291534558 ) ;
#6972 = DIRECTION ( 'NONE',  ( 0.000000000000000000, 0.000000000000000000, -1.000000000000000000 ) ) ;
#6973 = CARTESIAN_POINT ( 'NONE',  ( 27.00000000000000355, 1.649999999999999911, -11.18376618407356737 ) ) ;
#6974 = CIRCLE ( 'NONE', #3453, 24.00000000000000355 ) ;
#6975 = DIRECTION ( 'NONE',  ( 0.000000000000000000, 0.000000000000000000, -1.000000000000000000 ) ) ;
#6976 = ORIENTED_EDGE ( 'NONE', *, *, #368, .T. ) ;
#6977 = CARTESIAN_POINT ( 'NONE',  ( -16.57687742313193269, 99.99999999999998579, 15.91855687263828756 ) ) ;
#6978 = CARTESIAN_POINT ( 'NONE',  ( 8.122452352567329115, 100.0000000000000000, 21.04970292111833530 ) ) ;
#6979 = EDGE_CURVE ( 'NONE', #8050, #6810, #1962, .T. ) ;
#6980 = CARTESIAN_POINT ( 'NONE',  ( -1.128215178124998497, -3.328124999385482230, 1.954126010382872147 ) ) ;
#6981 = EDGE_LOOP ( 'NONE', ( #8333, #9810, #2671, #7708 ) ) ;
#6982 = ORIENTED_EDGE ( 'NONE', *, *, #4672, .T. ) ;
#6983 = EDGE_CURVE ( 'NONE', #10090, #5876, #9374, .T. ) ;
#6984 = PRODUCT_DEFINITION_FORMATION_WITH_SPECIFIED_SOURCE ( 'ANY', '', #668, .NOT_KNOWN. ) ;
#6985 = CARTESIAN_POINT ( 'NONE',  ( 1.128215178124999607, -1.753124999385482718, -1.954126010382871259 ) ) ;
#6986 = CARTESIAN_POINT ( 'NONE',  ( 1.653273178848927064E-15, 5.324999998907524734, -27.00000000000000355 ) ) ;
#6987 = CARTESIAN_POINT ( 'NONE',  ( 0.000000000000000000, 5.000000000000000000, -30.00000000000000000 ) ) ;
#6988 = AXIS2_PLACEMENT_3D ( 'NONE', #6628, #8943, #1135 ) ;
#6989 = CARTESIAN_POINT ( 'NONE',  ( 24.93339342948717885, 99.50000000000000000, -1.235376602564102644 ) ) ;
#6990 = CARTESIAN_POINT ( 'NONE',  ( 3.207968951880266761, 99.49999999999998579, -22.92616835434091627 ) ) ;
#6991 = CARTESIAN_POINT ( 'NONE',  ( 19.09188309203678102, 0.6999999999999999556, 19.09188309203678813 ) ) ;
#6992 =( BOUNDED_CURVE ( )  B_SPLINE_CURVE ( 2, ( #5126, #2835, #1206, #1156, #5290, #4345, #478, #3563, #8486 ),
 .UNSPECIFIED., .F., .T. ) 
 B_SPLINE_CURVE_WITH_KNOTS ( ( 3, 2, 2, 2, 3 ),
 ( 0.7291666666666667407, 0.7361111111111111605, 0.7500000000000000000, 0.7638888888888888395, 0.7708333333333333703 ),
 .UNSPECIFIED. ) 
 CURVE ( )  GEOMETRIC_REPRESENTATION_ITEM ( )  RATIONAL_B_SPLINE_CURVE ( ( 0.9330127018922192983, 0.9330127018922198534, 1.000000000000000000, 0.8660254037844387076, 1.000000000000000000, 0.8660254037844387076, 1.000000000000000000, 0.9330127018922187432, 0.9330127018922192983 ) ) 
 REPRESENTATION_ITEM ( '' )  );
#6993 = VERTEX_POINT ( 'NONE', #3670 ) ;
#6994 = CARTESIAN_POINT ( 'NONE',  ( 9.676361905416721143, 99.50000000000001421, 21.63547735782115566 ) ) ;
#6995 = CARTESIAN_POINT ( 'NONE',  ( 2.256430356250000546, -1.753124999385482718, 1.302750673588579877 ) ) ;
#6996 = AXIS2_PLACEMENT_3D ( 'NONE', #1070, #4314, #8981 ) ;
#6997 = CARTESIAN_POINT ( 'NONE',  ( -1.250000000000000222, -0.9187499987709658589, -2.165063509461096825 ) ) ;
#6998 = CARTESIAN_POINT ( 'NONE',  ( 9.357053078540884528, 100.0000000000000142, 19.70216357796830664 ) ) ;
#6999 = DIRECTION ( 'NONE',  ( 0.000000000000000000, -1.000000000000000000, 0.000000000000000000 ) ) ;
#7000 = VERTEX_POINT ( 'NONE', #10217 ) ;
#7001 = CARTESIAN_POINT ( 'NONE',  ( -16.61132721736409934, 99.50000000000001421, 16.61681399495993716 ) ) ;
#7002 = CARTESIAN_POINT ( 'NONE',  ( 27.43301269999999548, 1.099999998907525312, 11.36312591709337916 ) ) ;
#7003 = ORIENTED_EDGE ( 'NONE', *, *, #8620, .T. ) ;
#7004 = CARTESIAN_POINT ( 'NONE',  ( -2.500000000000000000, -4.949999999999999289, 0.000000000000000000 ) ) ;
#7005 = AXIS2_PLACEMENT_3D ( 'NONE', #7306, #880, #238 ) ;
#7006 = PLANE ( 'NONE',  #3416 ) ;
#7007 = CARTESIAN_POINT ( 'NONE',  ( 2.256430356250000546, -1.415624999385482807, 1.302750673588579877 ) ) ;
#7008 = ADVANCED_FACE ( 'NONE', ( #8536, #5284 ), #6231, .T. ) ;
#7009 = CARTESIAN_POINT ( 'NONE',  ( -27.43301270000000969, 4.699999998907524734, 11.36312591709335429 ) ) ;
#7010 = CARTESIAN_POINT ( 'NONE',  ( -27.43301270000000258, 1.549999998907525267, -3.359575119402369376E-15 ) ) ;
#7011 = VERTEX_POINT ( 'NONE', #1361 ) ;
#7012 = EDGE_CURVE ( 'NONE', #2877, #6069, #6176, .T. ) ;
#7013 = CARTESIAN_POINT ( 'NONE',  ( 9.778118981323553172, 99.99999999999998579, 20.11889122584574352 ) ) ;
#7014 = CARTESIAN_POINT ( 'NONE',  ( 5.243816414761435674, 99.50000000000000000, -23.48558366465980995 ) ) ;
#7015 = PLANE ( 'NONE',  #1940 ) ;
#7016 = CARTESIAN_POINT ( 'NONE',  ( 1.128215178124999607, -1.640624999385482896, -1.954126010382871259 ) ) ;
#7017 = CARTESIAN_POINT ( 'NONE',  ( -21.03505001771060634, 99.50000000000000000, -9.476849197711761263 ) ) ;
#7018 = EDGE_LOOP ( 'NONE', ( #1080, #9710, #10173, #1200, #5425, #4145, #8973, #7862, #9417, #4357, #6167, #5205 ) ) ;
#7019 = ORIENTED_EDGE ( 'NONE', *, *, #7028, .F. ) ;
#7020 = CARTESIAN_POINT ( 'NONE',  ( -1.595409442497313560E-16, -1.153124999385483074, -2.605501347177161087 ) ) ;
#7021 = CARTESIAN_POINT ( 'NONE',  ( 11.36312591709336850, 1.699999998907525178, 27.43301269999999903 ) ) ;
#7022 =( NAMED_UNIT ( * ) SI_UNIT ( $, .STERADIAN. ) SOLID_ANGLE_UNIT ( ) );
#7023 = VERTEX_POINT ( 'NONE', #4554 ) ;
#7024 = CARTESIAN_POINT ( 'NONE',  ( -15.10737684033046335, 99.99999999999995737, 15.12848924955281049 ) ) ;
#7025 = CARTESIAN_POINT ( 'NONE',  ( 1.653273178848927064E-15, 2.600000000000000533, -27.00000000000000355 ) ) ;
#7026 = CARTESIAN_POINT ( 'NONE',  ( 9.044794778432494908, 99.50000000000001421, 19.94873160813952140 ) ) ;
#7027 = ORIENTED_EDGE ( 'NONE', *, *, #10290, .T. ) ;
#7028 = EDGE_CURVE ( 'NONE', #7011, #9319, #8481, .T. ) ;
#7029 = CARTESIAN_POINT ( 'NONE',  ( -16.41302370085497131, 99.49999999999998579, 15.45185748370271206 ) ) ;
#7030 = CARTESIAN_POINT ( 'NONE',  ( 8.231219904624582639, 99.50000000000000000, 20.21381436664452735 ) ) ;
#7031 = CARTESIAN_POINT ( 'NONE',  ( 4.786228327491941173E-16, -5.090624999385482852, 2.605501347177161087 ) ) ;
#7032 = ORIENTED_EDGE ( 'NONE', *, *, #1705, .T. ) ;
#7033 = VERTEX_POINT ( 'NONE', #1419 ) ;
#7034 = ADVANCED_FACE ( 'NONE', ( #529, #1310 ), #4446, .F. ) ;
#7035 = CARTESIAN_POINT ( 'NONE',  ( -27.43301270000000258, 1.449999998907525178, -3.359575119402369376E-15 ) ) ;
#7036 = CARTESIAN_POINT ( 'NONE',  ( 2.500000000000000000, -0.2250000000000000056, -3.061616997868383141E-16 ) ) ;
#7037 =( GEOMETRIC_REPRESENTATION_CONTEXT ( 3 ) GLOBAL_UNCERTAINTY_ASSIGNED_CONTEXT ( ( #1416 ) ) GLOBAL_UNIT_ASSIGNED_CONTEXT ( ( #8634, #1458, #7842 ) ) REPRESENTATION_CONTEXT ( 'NONE', 'WORKASPACE' ) );
#7038 = CARTESIAN_POINT ( 'NONE',  ( -1.595409442497313560E-16, -2.615624999385482319, -2.605501347177161087 ) ) ;
#7039 = CARTESIAN_POINT ( 'NONE',  ( 5.207032889226773875, 99.50000000000000000, -23.83708953234284778 ) ) ;
#7040 = ADVANCED_FACE ( 'NONE', ( #3723 ), #7100, .T. ) ;
#7041 = LINE ( 'NONE', #6987, #9955 ) ;
#7042 = CARTESIAN_POINT ( 'NONE',  ( -1.249999999999998224, -1.668749998770965970, 2.165063509461097713 ) ) ;
#7043 = CARTESIAN_POINT ( 'NONE',  ( 4.200543313440712190, 100.0000000000000000, -21.13206004899810608 ) ) ;
#7044 = LINE ( 'NONE', #5377, #7614 ) ;
#7045 = CARTESIAN_POINT ( 'NONE',  ( -9.703070624755296135E-15, -4.331249998770966059, 2.500000000000000444 ) ) ;
#7046 = CARTESIAN_POINT ( 'NONE',  ( -2.256430356250000102, -1.078124999385482896, -1.302750673588580321 ) ) ;
#7047 = ORIENTED_EDGE ( 'NONE', *, *, #9051, .T. ) ;
#7048 = ADVANCED_FACE ( 'NONE', ( #740 ), #5606, .T. ) ;
#7049 = CARTESIAN_POINT ( 'NONE',  ( 0.000000000000000000, 0.000000000000000000, 1.622657008870242981E-16 ) ) ;
#7050 = CARTESIAN_POINT ( 'NONE',  ( 1.653273178848927064E-15, 5.599999997815050534, -27.00000000000000355 ) ) ;
#7051 =( BOUNDED_CURVE ( )  B_SPLINE_CURVE ( 2, ( #3593, #7877, #8352, #1183, #8673, #3959, #6930, #7560, #4692 ),
 .UNSPECIFIED., .F., .F. ) 
 B_SPLINE_CURVE_WITH_KNOTS ( ( 3, 2, 2, 2, 3 ),
 ( 0.6785714285714286031, 0.6964285714285713969, 0.7142857142857143016, 0.7321428571428570953, 0.7500000000000000000 ),
 .UNSPECIFIED. ) 
 CURVE ( )  GEOMETRIC_REPRESENTATION_ITEM ( )  RATIONAL_B_SPLINE_CURVE ( ( 1.000000000000000000, 0.9238795325112867385, 1.000000000000000000, 0.9238795325112867385, 1.000000000000000000, 0.9238795325112867385, 1.000000000000000000, 0.9238795325112867385, 1.000000000000000000 ) ) 
 REPRESENTATION_ITEM ( '' )  );
#7052 = DIRECTION ( 'NONE',  ( 1.000000000000000000, 0.000000000000000000, 0.000000000000000000 ) ) ;
#7053 = EDGE_LOOP ( 'NONE', ( #2295, #7491, #6982, #6573 ) ) ;
#7054 = CARTESIAN_POINT ( 'NONE',  ( -15.56095293356939813, 99.50000000000001421, 15.23332223661997453 ) ) ;
#7055 = CARTESIAN_POINT ( 'NONE',  ( -27.43301270000000258, 3.149999998907524912, -3.359575119402369376E-15 ) ) ;
#7056 = ORIENTED_EDGE ( 'NONE', *, *, #9765, .T. ) ;
#7057 = CARTESIAN_POINT ( 'NONE',  ( 5.302876193624534821E-16, -3.937500000000000444, 2.886751345948128655 ) ) ;
#7058 = CARTESIAN_POINT ( 'NONE',  ( -20.95611194834973645, 100.0000000000000000, -10.07788454426966318 ) ) ;
#7059 = CARTESIAN_POINT ( 'NONE',  ( -1.595409442497313560E-16, -3.965624999385482408, -2.605501347177161087 ) ) ;
#7060 = CARTESIAN_POINT ( 'NONE',  ( 27.00000000000000355, 0.5999999978150503122, 0.000000000000000000 ) ) ;
#7061 = CARTESIAN_POINT ( 'NONE',  ( 19.39806930854668110, 3.649999998907525356, -19.39806930854668110 ) ) ;
#7062 = PRODUCT_DEFINITION_CONTEXT ( 'detailed design', #865, 'design' ) ;
#7063 = CIRCLE ( 'NONE', #7548, 25.00000000000000000 ) ;
#7064 = CARTESIAN_POINT ( 'NONE',  ( -15.27171031718473770, 99.50000000000002842, 15.44886715306589764 ) ) ;
#7065 = B_SPLINE_CURVE_WITH_KNOTS ( 'NONE', 3,
 ( #10164, #7856, #3001, #7120, #6177, #7693, #7067, #6120, #5556, #6288, #9375, #9487, #5405, #8537, #5511 ),
 .UNSPECIFIED., .F., .F.,
 ( 4, 1, 1, 1, 1, 1, 1, 1, 1, 1, 1, 1, 4 ),
 ( 0.000000000000000000, 0.08963690308348271074, 0.1775767702671464110, 0.2649576542713044658, 0.3533131777157214604, 0.4402865524342069459, 0.5245518675747646853, 0.6066224975438009315, 0.6889424263984335051, 0.7698335385027974542, 0.8475882324521423206, 0.9236428641877653112, 1.000000000000000000 ),
 .UNSPECIFIED. ) ;
#7066 = CARTESIAN_POINT ( 'NONE',  ( 3.664124300404482337, 99.50000000000002842, -24.27219056640880623 ) ) ;
#7067 = CARTESIAN_POINT ( 'NONE',  ( 3.106448761625311139, 99.49999999999998579, -21.38062202216113761 ) ) ;
#7068 = DIRECTION ( 'NONE',  ( 0.05409991075415103434, 0.000000000000000000, 0.9985355274883277454 ) ) ;
#7069 = CARTESIAN_POINT ( 'NONE',  ( -1.128215178125000273, -2.465624999385482852, -1.954126010382871259 ) ) ;
#7070 = CARTESIAN_POINT ( 'NONE',  ( -21.69499712064247277, 99.49999999999998579, -9.295461156691713356 ) ) ;
#7071 = EDGE_LOOP ( 'NONE', ( #4368, #8839, #1798, #515, #8129, #6222, #6772, #4512, #2164, #9461, #4433, #9566, #3845, #1269, #7047, #9230, #1587, #5725, #3085, #8569, #5444, #10180, #5958, #160, #8623, #3128 ) ) ;
#7072 = CARTESIAN_POINT ( 'NONE',  ( -1.128215178125000273, -2.465624999385482852, -1.954126010382871259 ) ) ;
#7073 = CARTESIAN_POINT ( 'NONE',  ( -5.039362679103552881E-15, 0.9499999989075252893, 27.43301270000000258 ) ) ;
#7074 = VECTOR ( 'NONE', #7874, 1000.000000000000000 ) ;
#7075 = SURFACE_STYLE_FILL_AREA ( #4092 ) ;
#7076 = CARTESIAN_POINT ( 'NONE',  ( -15.07178375341841559, 99.99999999999997158, 15.16157792772069968 ) ) ;
#7077=STYLED_ITEM('',(#10387),#9927);
#7078 = CARTESIAN_POINT ( 'NONE',  ( 19.09188309203678813, 2.500000000000000000, -19.09188309203678813 ) ) ;
#7079 = CARTESIAN_POINT ( 'NONE',  ( 9.513000527211589841, 99.50000000000000000, 20.35102222961602436 ) ) ;
#7080 = ORIENTED_EDGE ( 'NONE', *, *, #8510, .F. ) ;
#7081 = CARTESIAN_POINT ( 'NONE',  ( -16.54770463920453949, 99.50000000000002842, 15.70234036036222847 ) ) ;
#7082 = CARTESIAN_POINT ( 'NONE',  ( 8.067960508813904141, 100.0000000000000000, 20.80952186068213905 ) ) ;
#7083 =( GEOMETRIC_REPRESENTATION_CONTEXT ( 3 ) GLOBAL_UNCERTAINTY_ASSIGNED_CONTEXT ( ( #1308 ) ) GLOBAL_UNIT_ASSIGNED_CONTEXT ( ( #6022, #4563, #7022 ) ) REPRESENTATION_CONTEXT ( 'NONE', 'WORKASPACE' ) );
#7084 = CARTESIAN_POINT ( 'NONE',  ( -1.128215178124998497, -3.778124999385482408, 1.954126010382872147 ) ) ;
#7085 = ORIENTED_EDGE ( 'NONE', *, *, #562, .F. ) ;
#7086 = CARTESIAN_POINT ( 'NONE',  ( -11.36312591709337561, 2.399999998907525356, 27.43301269999999548 ) ) ;
#7087 = CARTESIAN_POINT ( 'NONE',  ( 9.877377282685029372E-16, -1.687499999999999778, 2.500000000000000000 ) ) ;
#7088 = EDGE_CURVE ( 'NONE', #10177, #1260, #8699, .T. ) ;
#7089 = CARTESIAN_POINT ( 'NONE',  ( -2.256430356250000102, -0.2906249993854829183, -1.302750673588580321 ) ) ;
#7090 = CARTESIAN_POINT ( 'NONE',  ( -16.37951318544778445, 99.99999999999997158, 15.41600550949200077 ) ) ;
#7091 = ORIENTED_EDGE ( 'NONE', *, *, #8252, .T. ) ;
#7092 = CARTESIAN_POINT ( 'NONE',  ( 4.486604876299897349, 99.99999999999997158, -21.85617661337775885 ) ) ;
#7093 = ORIENTED_EDGE ( 'NONE', *, *, #1121, .T. ) ;
#7094 = CARTESIAN_POINT ( 'NONE',  ( 2.500000000000000000, -1.068749998770965881, -3.061616997868383141E-16 ) ) ;
#7095 = VERTEX_POINT ( 'NONE', #8849 ) ;
#7096 = CARTESIAN_POINT ( 'NONE',  ( 6.123233995736709336E-17, 0.000000000000000000, 0.4999999999999953371 ) ) ;
#7097 = CARTESIAN_POINT ( 'NONE',  ( -15.72775836928289017, 100.0000000000000000, 17.03252426573849476 ) ) ;
#7098 = CARTESIAN_POINT ( 'NONE',  ( -2.499999999999999112, -4.406249998770965348, 1.443375672974065882 ) ) ;
#7099 = CARTESIAN_POINT ( 'NONE',  ( -1.595409442497313560E-16, -1.603124999385482807, -2.605501347177161087 ) ) ;
#7100 = B_SPLINE_SURFACE_WITH_KNOTS ( 'NONE', 3, 1, ( 
 ( #474, #6905 ),
 ( #632, #9432 ),
 ( #3830, #10102 ),
 ( #7634, #2258 ),
 ( #4666, #2938 ),
 ( #8648, #2831 ),
 ( #3878, #9204 ),
 ( #3933, #5510 ),
 ( #7066, #10320 ),
 ( #4817, #3203 ),
 ( #9679, #9534 ),
 ( #1624, #3157 ),
 ( #5709, #9486 ),
 ( #7172, #2518 ),
 ( #7907, #9579 ),
 ( #7217, #6340 ),
 ( #4915, #6438 ),
 ( #6488, #4714 ),
 ( #9630, #7119 ) ),
 .UNSPECIFIED., .F., .F., .F.,
 ( 4, 1, 1, 1, 1, 1, 1, 1, 1, 1, 1, 1, 1, 1, 1, 1, 4 ),
 ( 2, 2 ),
 ( 0.000000000000000000, 0.07313710028058939550, 0.1429478298248799129, 0.2105045057187734658, 0.2751999312753631854, 0.3390602298032547868, 0.4018764873508149926, 0.4650016082884899093, 0.5281538368899733049, 0.5906348070863262079, 0.6510495490485337378, 0.7103018853965116230, 0.7674338915725752441, 0.8249350906448947862, 0.8823686014076175255, 0.9405824579944982444, 1.000000000000000000 ),
 ( 0.000000000000000000, 1.000000000000000000 ),
 .UNSPECIFIED. ) ;
#7101 = ORIENTED_EDGE ( 'NONE', *, *, #3786, .T. ) ;
#7102 = LINE ( 'NONE', #4022, #6940 ) ;
#7103 = VECTOR ( 'NONE', #6698, 1000.000000000000000 ) ;
#7104 = DIRECTION ( 'NONE',  ( -0.000000000000000000, 0.000000000000000000, 1.000000000000000000 ) ) ;
#7105 = EDGE_CURVE ( 'NONE', #3531, #6494, #8013, .T. ) ;
#7106 = ORIENTED_EDGE ( 'NONE', *, *, #5617, .T. ) ;
#7107 = CARTESIAN_POINT ( 'NONE',  ( -16.30857500771091040, 99.99999999999994316, 15.34700649443169063 ) ) ;
#7108 = AXIS2_PLACEMENT_3D ( 'NONE', #4961, #4279, #7320 ) ;
#7109 = CARTESIAN_POINT ( 'NONE',  ( 1.679787559701184688E-15, 4.549999998907526155, -27.43301270000000258 ) ) ;
#7110 = EDGE_LOOP ( 'NONE', ( #8997, #2447, #1563, #8455 ) ) ;
#7111 = EDGE_CURVE ( 'NONE', #7619, #3366, #8684, .T. ) ;
#7112 = CARTESIAN_POINT ( 'NONE',  ( -2.500000000000000000, -3.637499999999999734, -1.443375672974064106 ) ) ;
#7113 = CIRCLE ( 'NONE', #3594, 23.99999999999999645 ) ;
#7114 = CARTESIAN_POINT ( 'NONE',  ( 3.374624233514611937, 99.50000000000002842, -23.25900349070959550 ) ) ;
#7115 = CARTESIAN_POINT ( 'NONE',  ( 1.128215178124999607, -3.553124999385482319, -1.954126010382871259 ) ) ;
#7116 = CARTESIAN_POINT ( 'NONE',  ( -20.97746206809550884, 100.0000000000000000, -11.22189255051946688 ) ) ;
#7117 = CARTESIAN_POINT ( 'NONE',  ( -27.43301270000000969, 4.799999998907525267, 11.36312591709335429 ) ) ;
#7118 = DIRECTION ( 'NONE',  ( 0.9853569121566161382, 0.000000000000000000, 0.1705044153832351028 ) ) ;
#7119 = CARTESIAN_POINT ( 'NONE',  ( 3.282077632710153292, 100.0000000000000000, -23.74569985055724786 ) ) ;
#7120 = CARTESIAN_POINT ( 'NONE',  ( 3.428579745388047328, 99.49999999999998579, -21.16399209792802694 ) ) ;
#7121 = DIRECTION ( 'NONE',  ( -0.000000000000000000, -1.000000000000000000, 0.000000000000000000 ) ) ;
#7122 = CARTESIAN_POINT ( 'NONE',  ( -2.256430356250000102, -2.840624999385482852, 0.000000000000000000 ) ) ;
#7123 = CARTESIAN_POINT ( 'NONE',  ( -21.59614764830937972, 99.50000000000001421, -9.292069227195950631 ) ) ;
#7124 = ORIENTED_EDGE ( 'NONE', *, *, #9346, .F. ) ;
#7125 = CARTESIAN_POINT ( 'NONE',  ( 4.786228327491941173E-16, -3.178124999385482763, 2.605501347177161087 ) ) ;
#7126 = CARTESIAN_POINT ( 'NONE',  ( 27.43301270000000258, 0.3499999989075252005, 0.000000000000000000 ) ) ;
#7127 = CYLINDRICAL_SURFACE ( 'NONE', #4588, 2.500000000000000000 ) ;
#7128 = CARTESIAN_POINT ( 'NONE',  ( -19.09188309203678813, 1.300000000000000266, 19.09188309203678457 ) ) ;
#7129 = CARTESIAN_POINT ( 'NONE',  ( 2.500000000000000000, -3.281249998770965792, -1.443375672974065438 ) ) ;
#7130 = ORIENTED_EDGE ( 'NONE', *, *, #3912, .T. ) ;
#7131 = AXIS2_PLACEMENT_3D ( 'NONE', #7665, #10135, #10074 ) ;
#7132 = FACE_OUTER_BOUND ( 'NONE', #9152, .T. ) ;
#7133 = CARTESIAN_POINT ( 'NONE',  ( -20.96643530928959365, 99.99999999999997158, -10.05541671241504886 ) ) ;
#7134 = VERTEX_POINT ( 'NONE', #1572 ) ;
#7135 = CARTESIAN_POINT ( 'NONE',  ( -1.128215178125000273, -3.928124999385483207, -1.954126010382871259 ) ) ;
#7136 = DIRECTION ( 'NONE',  ( -0.3923910917372159246, 0.000000000000000000, -0.9197984731044490658 ) ) ;
#7137 = CARTESIAN_POINT ( 'NONE',  ( -27.43301270000000258, 2.249999998907525001, -3.359575119402369376E-15 ) ) ;
#7138 = CARTESIAN_POINT ( 'NONE',  ( 3.472565890032746960, 99.50000000000002842, -24.54662015932514052 ) ) ;
#7139 = CARTESIAN_POINT ( 'NONE',  ( -22.55793349878803156, 99.50000000000000000, -10.88926985104519929 ) ) ;
#7140 = VECTOR ( 'NONE', #3707, 1000.000000000000000 ) ;
#7141 = CARTESIAN_POINT ( 'NONE',  ( 4.786228327491940187E-16, -4.190624999385482496, 2.605501347177161087 ) ) ;
#7142 = CARTESIAN_POINT ( 'NONE',  ( -16.54512803120131181, 100.0000000000000000, 16.13427955854364626 ) ) ;
#7143 = CARTESIAN_POINT ( 'NONE',  ( 9.873655262861264603, 99.99999999999998579, 20.34710108723753308 ) ) ;
#7144 = CARTESIAN_POINT ( 'NONE',  ( 4.405197143102897783, 99.99999999999994316, -21.72932741277565682 ) ) ;
#7145 = EDGE_CURVE ( 'NONE', #463, #4730, #3105, .T. ) ;
#7146 =( GEOMETRIC_REPRESENTATION_CONTEXT ( 3 ) GLOBAL_UNCERTAINTY_ASSIGNED_CONTEXT ( ( #4033 ) ) GLOBAL_UNIT_ASSIGNED_CONTEXT ( ( #5013, #8999, #8263 ) ) REPRESENTATION_CONTEXT ( 'NONE', 'WORKASPACE' ) );
#7147 = CARTESIAN_POINT ( 'NONE',  ( 2.500000000000000000, -3.281249998770965792, -1.443375672974064994 ) ) ;
#7148 = ORIENTED_EDGE ( 'NONE', *, *, #5503, .F. ) ;
#7149 = CARTESIAN_POINT ( 'NONE',  ( 4.723706824522782455, 100.0000000000000142, -24.08630974238606370 ) ) ;
#7150 = CARTESIAN_POINT ( 'NONE',  ( 2.939152317953648289E-15, 87.00000000000001421, 24.00000000000000355 ) ) ;
#7151 = DIRECTION ( 'NONE',  ( -0.000000000000000000, -1.000000000000000000, 0.000000000000000000 ) ) ;
#7152 = CARTESIAN_POINT ( 'NONE',  ( 1.128215178124999607, -4.790624999385483029, -1.954126010382871259 ) ) ;
#7153 = EDGE_CURVE ( 'NONE', #3495, #7824, #794, .T. ) ;
#7154 = ORIENTED_EDGE ( 'NONE', *, *, #3072, .F. ) ;
#7155 = DIRECTION ( 'NONE',  ( 0.000000000000000000, 0.000000000000000000, -1.000000000000000000 ) ) ;
#7156 = AXIS2_PLACEMENT_3D ( 'NONE', #2189, #2011, #8522 ) ;
#7157 = EDGE_CURVE ( 'NONE', #906, #9263, #3648, .T. ) ;
#7158 = CARTESIAN_POINT ( 'NONE',  ( -22.21584973381871464, 99.50000000000001421, -9.938501092090024969 ) ) ;
#7159 = CARTESIAN_POINT ( 'NONE',  ( 9.446088657802272692, 100.0000000000000426, 20.22669104216016578 ) ) ;
#7160 = VERTEX_POINT ( 'NONE', #6386 ) ;
#7161 = AXIS2_PLACEMENT_3D ( 'NONE', #9932, #8360, #1915 ) ;
#7162 = EDGE_CURVE ( 'NONE', #8581, #1470, #976, .T. ) ;
#7163 = CARTESIAN_POINT ( 'NONE',  ( -2.500000000000000000, -4.087500000000000355, -1.443375672974064106 ) ) ;
#7164 = CARTESIAN_POINT ( 'NONE',  ( -2.500000000000000000, -0.4312499987709658700, -1.443375672974064106 ) ) ;
#7165 = CARTESIAN_POINT ( 'NONE',  ( 2.256430356250000102, -4.978124999385482141, -2.763330213280484622E-16 ) ) ;
#7166 = ADVANCED_FACE ( 'NONE', ( #3250 ), #9355, .T. ) ;
#7167 = CARTESIAN_POINT ( 'NONE',  ( -21.30928386698190025, 99.50000000000000000, -11.02857376369709996 ) ) ;
#7168 = CARTESIAN_POINT ( 'NONE',  ( -27.00000000000001421, 1.049999997815050490, 11.18376618407356382 ) ) ;
#7169 = UNCERTAINTY_MEASURE_WITH_UNIT (LENGTH_MEASURE( 1.000000000000000082E-05 ), #1688, 'distance_accuracy_value', 'NONE');
#7170 = CARTESIAN_POINT ( 'NONE',  ( -15.13293277027690209, 99.99999999999997158, 16.13104881108577970 ) ) ;
#7171 = ADVANCED_FACE ( 'NONE', ( #5056 ), #9507, .T. ) ;
#7172 = CARTESIAN_POINT ( 'NONE',  ( 3.386276725104728769, 99.50000000000001421, -24.01678749451497907 ) ) ;
#7173 = CARTESIAN_POINT ( 'NONE',  ( -16.05266356869597644, 99.50000000000000000, 16.62382211633880047 ) ) ;
#7174 = CARTESIAN_POINT ( 'NONE',  ( 7.500000000000000000, 105.0000000000000142, 1.000000000000000222 ) ) ;
#7175 = CARTESIAN_POINT ( 'NONE',  ( 1.128215178124999607, -4.340624999385482852, -1.954126010382871259 ) ) ;
#7176 = CARTESIAN_POINT ( 'NONE',  ( -20.95972469638759250, 99.50000000000000000, -9.536167108072199028 ) ) ;
#7177 = VERTEX_POINT ( 'NONE', #4136 ) ;
#7178 = CARTESIAN_POINT ( 'NONE',  ( 4.786228327491941173E-16, -1.378124999385482941, 2.605501347177161087 ) ) ;
#7179 = CARTESIAN_POINT ( 'NONE',  ( 11.36312591709336850, 4.899999998907526688, 27.43301269999999903 ) ) ;
#7180 = DIRECTION ( 'NONE',  ( -0.000000000000000000, 1.000000000000000000, -0.000000000000000000 ) ) ;
#7181 = CARTESIAN_POINT ( 'NONE',  ( 1.653273178848927064E-15, 3.400000000000000355, -27.00000000000000355 ) ) ;
#7182 = CARTESIAN_POINT ( 'NONE',  ( 3.298672054714395063, 100.0000000000000142, -22.72039518595936869 ) ) ;
#7183 = ADVANCED_FACE ( 'NONE', ( #6676 ), #7462, .F. ) ;
#7184 =( NAMED_UNIT ( * ) SI_UNIT ( $, .STERADIAN. ) SOLID_ANGLE_UNIT ( ) );
#7185 = CARTESIAN_POINT ( 'NONE',  ( -2.500000000000000000, -0.1968749993854829461, 0.000000000000000000 ) ) ;
#7186 = ORIENTED_EDGE ( 'NONE', *, *, #191, .F. ) ;
#7187 = CARTESIAN_POINT ( 'NONE',  ( -2.256430356249999214, -3.365624999385482319, 1.302750673588581876 ) ) ;
#7188 = CARTESIAN_POINT ( 'NONE',  ( 27.00000000000000355, 0.05000000000000000278, -11.18376618407356915 ) ) ;
#7189 = CARTESIAN_POINT ( 'NONE',  ( -11.36312591709337561, 1.599999998907525756, 27.43301269999999548 ) ) ;
#7190 = CARTESIAN_POINT ( 'NONE',  ( 4.241330131419338123, 99.99999999999998579, -24.68798891778770965 ) ) ;
#7191 = PRODUCT_DEFINITION_SHAPE ( 'NONE', 'NONE',  #3442 ) ;
#7192 = CARTESIAN_POINT ( 'NONE',  ( -27.00000000000001421, 1.049999997815050490, 11.18376618407356560 ) ) ;
#7193 = CARTESIAN_POINT ( 'NONE',  ( 1.128215178125001161, -3.253124999385482496, 1.954126010382870815 ) ) ;
#7194 = DIRECTION ( 'NONE',  ( -0.9197984731044490658, 0.000000000000000000, 0.3923910917372159246 ) ) ;
#7195 = CARTESIAN_POINT ( 'NONE',  ( -22.33111803333905243, 99.99999999999997158, -9.558150950182401573 ) ) ;
#7196 = CARTESIAN_POINT ( 'NONE',  ( 1.653273178848927064E-15, 5.599999997815050534, -27.00000000000000355 ) ) ;
#7197 = CARTESIAN_POINT ( 'NONE',  ( 2.500000000000000444, -3.356249998770965082, 1.443375672974063439 ) ) ;
#7198 = VECTOR ( 'NONE', #8784, 1000.000000000000000 ) ;
#7199 = CARTESIAN_POINT ( 'NONE',  ( 1.653273178848927064E-15, 4.200000000000000178, -27.00000000000000355 ) ) ;
#7200 = CARTESIAN_POINT ( 'NONE',  ( -15.45548338988150938, 99.99999999999997158, 16.93306818456458984 ) ) ;
#7201 = DIRECTION ( 'NONE',  ( -0.5137073458062109133, 0.000000000000000000, -0.8579654788304353907 ) ) ;
#7202 = CARTESIAN_POINT ( 'NONE',  ( 1.128215178125001161, -4.940624999385482496, 1.954126010382870815 ) ) ;
#7203 = ADVANCED_FACE ( 'NONE', ( #3542 ), #4469, .T. ) ;
#7204 = DIRECTION ( 'NONE',  ( 0.000000000000000000, 1.000000000000000000, 0.000000000000000000 ) ) ;
#7205 = CARTESIAN_POINT ( 'NONE',  ( -2.500000000000000000, -3.581249998770966059, -1.443375672974064106 ) ) ;
#7206 = CARTESIAN_POINT ( 'NONE',  ( 26.99999999999999645, 2.949999997815051067, 11.18376618407358691 ) ) ;
#7207 = CARTESIAN_POINT ( 'NONE',  ( 27.43301269999999548, 5.099999998907525089, 11.36312591709337916 ) ) ;
#7208 = ORIENTED_EDGE ( 'NONE', *, *, #3581, .T. ) ;
#7209 = PRESENTATION_STYLE_ASSIGNMENT (( #2601 ) ) ;
#7210 = EDGE_CURVE ( 'NONE', #906, #2131, #1761, .T. ) ;
#7211 = CARTESIAN_POINT ( 'NONE',  ( 2.852289972453743161, 99.99999999999997158, -22.14293542748032451 ) ) ;
#7212 = CARTESIAN_POINT ( 'NONE',  ( 1.128215178125001161, -4.153124999385482852, 1.954126010382870815 ) ) ;
#7213 = CARTESIAN_POINT ( 'NONE',  ( -20.79740905086423552, 100.0000000000000142, -11.06234285579171051 ) ) ;
#7214 = CARTESIAN_POINT ( 'NONE',  ( 19.09188309203678813, 1.499999997815050223, -19.09188309203678813 ) ) ;
#7215 = CARTESIAN_POINT ( 'NONE',  ( -15.11611088805441661, 99.99999999999997158, 16.06180012866831319 ) ) ;
#7216 = VECTOR ( 'NONE', #5249, 1000.000000000000114 ) ;
#7217 = CARTESIAN_POINT ( 'NONE',  ( 3.320270046935387853, 99.49999999999998579, -23.88810568987970484 ) ) ;
#7218 = CARTESIAN_POINT ( 'NONE',  ( 3.611424427577684781, 100.0000000000000142, -21.45475674085064099 ) ) ;
#7219 = CIRCLE ( 'NONE', #8898, 23.99999999999999645 ) ;
#7220 = LINE ( 'NONE', #54, #621 ) ;
#7221 = CARTESIAN_POINT ( 'NONE',  ( -1.128215178124998497, -4.565624999385482496, 1.954126010382872147 ) ) ;
#7222 = CARTESIAN_POINT ( 'NONE',  ( 3.286905236079108672, 99.50000000000004263, -23.77014634954566574 ) ) ;
#7223 = ORIENTED_EDGE ( 'NONE', *, *, #8265, .F. ) ;
#7224 = ORIENTED_EDGE ( 'NONE', *, *, #8122, .F. ) ;
#7225 = CARTESIAN_POINT ( 'NONE',  ( -2.256430356250000102, -1.040624999385483029, 0.000000000000000000 ) ) ;
#7226 = CARTESIAN_POINT ( 'NONE',  ( 27.43301269999999548, 1.099999998907525089, 11.36312591709337738 ) ) ;
#7227 =( NAMED_UNIT ( * ) SI_UNIT ( $, .STERADIAN. ) SOLID_ANGLE_UNIT ( ) );
#7228 = DIRECTION ( 'NONE',  ( 0.000000000000000000, -1.000000000000000000, 0.000000000000000000 ) ) ;
#7229 = CARTESIAN_POINT ( 'NONE',  ( 27.43301270000000258, 1.049999998907525267, 0.000000000000000000 ) ) ;
#7230 = CARTESIAN_POINT ( 'NONE',  ( 1.249999999999999334, -3.243749998770965259, -2.165063509461096825 ) ) ;
#7231 = CARTESIAN_POINT ( 'NONE',  ( 1.034219503716432668E-14, -3.262500000000000178, -2.500000000000000000 ) ) ;
#7232 = LINE ( 'NONE', #860, #8739 ) ;
#7233 = CARTESIAN_POINT ( 'NONE',  ( 4.739008722453744049, 99.50000000000001421, -24.06821587619827696 ) ) ;
#7234 = CARTESIAN_POINT ( 'NONE',  ( 2.500000000000000000, -5.118749998770964815, -3.061616997868383141E-16 ) ) ;
#7235 = B_SPLINE_CURVE_WITH_KNOTS ( 'NONE', 3,
 ( #1050, #7423, #5123, #5861, #1098, #3615, #4293, #6797, #1926, #4341, #8957 ),
 .UNSPECIFIED., .F., .F.,
 ( 4, 1, 1, 1, 1, 1, 1, 1, 4 ),
 ( 0.000000000000000000, 0.1199228846740813259, 0.2396820999030742083, 0.3587608595380448184, 0.4799620281296770319, 0.6043577515038436321, 0.7314057062717854718, 0.8632643124108332344, 1.000000000000000000 ),
 .UNSPECIFIED. ) ;
#7236 = CARTESIAN_POINT ( 'NONE',  ( -5.039362679103552881E-15, 1.649999998907525356, 27.43301270000000258 ) ) ;
#7237 = STYLED_ITEM ( 'NONE', ( #2042 ), #6379 ) ;
#7238 = CARTESIAN_POINT ( 'NONE',  ( -27.00000000000000355, 1.950000000000000400, -11.18376618407357270 ) ) ;
#7239 = EDGE_CURVE ( 'NONE', #3171, #471, #9855, .T. ) ;
#7240 = CARTESIAN_POINT ( 'NONE',  ( -22.22752541189434794, 99.99999999999994316, -11.26717589342885084 ) ) ;
#7241 = CARTESIAN_POINT ( 'NONE',  ( -1.595409442497313560E-16, -3.965624999385482408, -2.605501347177161087 ) ) ;
#7242 = DIRECTION ( 'NONE',  ( -0.000000000000000000, 1.000000000000000000, -0.000000000000000000 ) ) ;
#7243 = CARTESIAN_POINT ( 'NONE',  ( -22.21668755910108928, 100.0000000000000426, -9.472979539922778969 ) ) ;
#7244 = CARTESIAN_POINT ( 'NONE',  ( 27.00000000000000355, 5.449999997815051067, -11.18376618407356915 ) ) ;
#7245 = VECTOR ( 'NONE', #7980, 1000.000000000000000 ) ;
#7246 = CARTESIAN_POINT ( 'NONE',  ( 1.249999999999999334, -4.143749998770966059, -2.165063509461096825 ) ) ;
#7247 = ORIENTED_EDGE ( 'NONE', *, *, #5805, .F. ) ;
#7248 = DIRECTION ( 'NONE',  ( -0.000000000000000000, -1.000000000000000000, -0.000000000000000000 ) ) ;
#7249 = LINE ( 'NONE', #2339, #3132 ) ;
#7250 = CARTESIAN_POINT ( 'NONE',  ( -21.86704275050744073, 99.50000000000001421, -11.06111336656620026 ) ) ;
#7251 = CARTESIAN_POINT ( 'NONE',  ( 1.128215178125001161, -3.140624999385482674, 1.954126010382870815 ) ) ;
#7252 = CARTESIAN_POINT ( 'NONE',  ( -22.31427554260534052, 100.0000000000000284, -10.13077409178744404 ) ) ;
#7253 = CARTESIAN_POINT ( 'NONE',  ( -15.26676860252058887, 99.49999999999998579, 16.38168943497750973 ) ) ;
#7254 = CARTESIAN_POINT ( 'NONE',  ( -22.00707282958688182, 99.49999999999997158, -9.748971510896797810 ) ) ;
#7255 = CARTESIAN_POINT ( 'NONE',  ( -27.00000000000000355, 2.549999997815050712, -11.18376618407357270 ) ) ;
#7256 = CARTESIAN_POINT ( 'NONE',  ( -27.43301270000000969, 3.199999998907525622, 11.36312591709335784 ) ) ;
#7257 = ORIENTED_EDGE ( 'NONE', *, *, #5311, .T. ) ;
#7258 = CARTESIAN_POINT ( 'NONE',  ( 4.277141017070624329, 99.50000000000002842, -21.57940364907851816 ) ) ;
#7259 = AXIS2_PLACEMENT_3D ( 'NONE', #4622, #8658, #3787 ) ;
#7260 = CARTESIAN_POINT ( 'NONE',  ( 3.277744210708366079, 99.99999999999998579, -23.71256836663369327 ) ) ;
#7261 = CARTESIAN_POINT ( 'NONE',  ( -1.728525935690056192, -5.253648612710515309, -1.450405475118361043 ) ) ;
#7262 = DIRECTION ( 'NONE',  ( -1.000000000000000000, 0.000000000000000000, 0.000000000000000000 ) ) ;
#7263 = CARTESIAN_POINT ( 'NONE',  ( 19.39806930854667399, 5.049999998907525267, 19.39806930854668465 ) ) ;
#7264 = CARTESIAN_POINT ( 'NONE',  ( -15.10687288066601930, 99.99999999999995737, 15.84109048427130517 ) ) ;
#7265 = AXIS2_PLACEMENT_3D ( 'NONE', #8306, #8114, #4917 ) ;
#7266 = DIRECTION ( 'NONE',  ( -0.8799640205556051864, 0.000000000000000000, -0.4750403377899758417 ) ) ;
#7267 = DIRECTION ( 'NONE',  ( 0.000000000000000000, -1.000000000000000000, 0.000000000000000000 ) ) ;
#7268 = ADVANCED_FACE ( 'NONE', ( #4180 ), #1240, .T. ) ;
#7269 = PRODUCT ( 'Reservoir Tank', 'Reservoir Tank', '', ( #522 ) ) ;
#7270 = DIRECTION ( 'NONE',  ( 0.000000000000000000, -1.000000000000000000, 0.000000000000000000 ) ) ;
#7271 = CARTESIAN_POINT ( 'NONE',  ( 2.256430356250000546, -4.003124999385482496, 1.302750673588579877 ) ) ;
#7272 = CARTESIAN_POINT ( 'NONE',  ( 9.676361905416721143, 100.0000000000000142, 21.63547735782115566 ) ) ;
#7273 = ORIENTED_EDGE ( 'NONE', *, *, #4019, .T. ) ;
#7274 = AXIS2_PLACEMENT_3D ( 'NONE', #5519, #1685, #8072 ) ;
#7275 = VERTEX_POINT ( 'NONE', #5209 ) ;
#7276 = CARTESIAN_POINT ( 'NONE',  ( 2.256430356249999658, -3.928124999385482319, -1.302750673588581432 ) ) ;
#7277 = CARTESIAN_POINT ( 'NONE',  ( -5.039362679103552881E-15, 4.049999998907525267, 27.43301270000000258 ) ) ;
#7278 = CARTESIAN_POINT ( 'NONE',  ( 24.93339342948717885, 100.0000000000000000, -1.235376602564102644 ) ) ;
#7279 = B_SPLINE_CURVE_WITH_KNOTS ( 'NONE', 3,
 ( #9339, #2169, #9124, #1943, #5138, #5352, #5970, #2726, #6126, #535, #5177, #2153, #9262, #8542, #6801 ),
 .UNSPECIFIED., .F., .F.,
 ( 4, 1, 1, 1, 1, 1, 1, 1, 1, 1, 1, 1, 4 ),
 ( 0.000000000000000000, 0.08450893420292937552, 0.1670077533940913517, 0.2489527561816328172, 0.3323249201989921797, 0.4152786837838207679, 0.4972150204155297848, 0.5791806016509544186, 0.6636863847498374325, 0.7483757861910059761, 0.8320455266939520422, 0.9153409992114193150, 1.000000000000000000 ),
 .UNSPECIFIED. ) ;
#7280 = CARTESIAN_POINT ( 'NONE',  ( 27.00000000000000355, 4.849999999999999645, -11.18376618407356737 ) ) ;
#7281 = CARTESIAN_POINT ( 'NONE',  ( -16.33590634957226229, 100.0000000000000000, 16.80570853669505382 ) ) ;
#7282 = VERTEX_POINT ( 'NONE', #6889 ) ;
#7283 = CYLINDRICAL_SURFACE ( 'NONE', #814, 17.50000000000000355 ) ;
#7284 = LINE ( 'NONE', #1776, #9409 ) ;
#7285 = ADVANCED_FACE ( 'NONE', ( #2922 ), #1188, .F. ) ;
#7286 = AXIS2_PLACEMENT_3D ( 'NONE', #3075, #9401, #8621 ) ;
#7287 = CARTESIAN_POINT ( 'NONE',  ( -9.703070624755296135E-15, -5.231249998770965526, 2.500000000000000444 ) ) ;
#7288 = CARTESIAN_POINT ( 'NONE',  ( 0.000000000000000000, 0.000000000000000000, -2.500000000000000000 ) ) ;
#7289 = CARTESIAN_POINT ( 'NONE',  ( 3.538198506519217190, 99.49999999999998579, -24.58220198924426114 ) ) ;
#7290 = CARTESIAN_POINT ( 'NONE',  ( 24.91446314102564230, 100.0000000000000000, -1.581029647435897578 ) ) ;
#7291 = CARTESIAN_POINT ( 'NONE',  ( 2.256430356250000546, -3.665624999385482585, 1.302750673588579877 ) ) ;
#7292 = LINE ( 'NONE', #765, #8061 ) ;
#7293 = CARTESIAN_POINT ( 'NONE',  ( -22.69253165798458127, 99.50000000000001421, -10.28928739654909563 ) ) ;
#7294 = PRODUCT_RELATED_PRODUCT_CATEGORY ( 'part', '', ( #668 ) ) ;
#7295 = DIRECTION ( 'NONE',  ( 1.000000000000000000, 0.000000000000000000, -0.000000000000000000 ) ) ;
#7296 = ADVANCED_FACE ( 'NONE', ( #4379 ), #4431, .T. ) ;
#7297 = EDGE_CURVE ( 'NONE', #2978, #4542, #6105, .T. ) ;
#7298 = CARTESIAN_POINT ( 'NONE',  ( -2.500000000000000000, -4.893749998770965171, 0.000000000000000000 ) ) ;
#7299 = ORIENTED_EDGE ( 'NONE', *, *, #8716, .T. ) ;
#7300 = VECTOR ( 'NONE', #5737, 1000.000000000000114 ) ;
#7301 = CARTESIAN_POINT ( 'NONE',  ( 3.712044765110731337, 99.99999999999998579, -21.08683700305641651 ) ) ;
#7302 = CARTESIAN_POINT ( 'NONE',  ( 3.000000000000000000, -15.00000000000000000, 1.732050807568879192 ) ) ;
#7303 = CARTESIAN_POINT ( 'NONE',  ( -14.79004890936967875, 99.99999999999998579, 16.19006955939758541 ) ) ;
#7304 = CARTESIAN_POINT ( 'NONE',  ( 1.128215178124999607, -2.990624999385482763, -1.954126010382871259 ) ) ;
#7305 = EDGE_LOOP ( 'NONE', ( #1235, #2836, #1423, #8219 ) ) ;
#7306 = CARTESIAN_POINT ( 'NONE',  ( 0.000000000000000000, -25.00000000000000000, 0.000000000000000000 ) ) ;
#7307 = CARTESIAN_POINT ( 'NONE',  ( -7.500000000000000000, 104.5000000000000142, 1.000000000000000222 ) ) ;
#7308 = PLANE ( 'NONE',  #3970 ) ;
#7309 = CARTESIAN_POINT ( 'NONE',  ( 8.612131858919537919, 99.99999999999998579, 19.96100069886393413 ) ) ;
#7310 = EDGE_LOOP ( 'NONE', ( #8470, #3526, #3697, #6228 ) ) ;
#7311 = CARTESIAN_POINT ( 'NONE',  ( 4.486604876299897349, 99.50000000000000000, -21.85617661337775885 ) ) ;
#7312 =( GEOMETRIC_REPRESENTATION_CONTEXT ( 3 ) GLOBAL_UNCERTAINTY_ASSIGNED_CONTEXT ( ( #791 ) ) GLOBAL_UNIT_ASSIGNED_CONTEXT ( ( #10331, #8804, #7227 ) ) REPRESENTATION_CONTEXT ( 'NONE', 'WORKASPACE' ) );
#7313 = CARTESIAN_POINT ( 'NONE',  ( 3.573144549190039321, 99.49999999999998579, -23.04580706645134214 ) ) ;
#7314 = CARTESIAN_POINT ( 'NONE',  ( 5.725936192474917696, 100.0000000000000000, 21.08018326417248645 ) ) ;
#7315 = CARTESIAN_POINT ( 'NONE',  ( -20.88772068548257366, 100.0000000000000142, -11.14739719174079546 ) ) ;
#7316 = CARTESIAN_POINT ( 'NONE',  ( 27.00000000000000355, 0.5999999978150503122, 0.000000000000000000 ) ) ;
#7317 = CARTESIAN_POINT ( 'NONE',  ( 19.09188309203678102, 3.100000000000000533, 19.09188309203678813 ) ) ;
#7318 = CARTESIAN_POINT ( 'NONE',  ( 0.6698729810778112359, -4.576346188203299192, -2.499999999999996447 ) ) ;
#7319 = CARTESIAN_POINT ( 'NONE',  ( -15.49014769301379069, 99.49999999999997158, 16.56834637662448273 ) ) ;
#7320 = DIRECTION ( 'NONE',  ( 4.336808689942017736E-16, 0.000000000000000000, -1.000000000000000000 ) ) ;
#7321 = VECTOR ( 'NONE', #7375, 1000.000000000000114 ) ;
#7322 = CARTESIAN_POINT ( 'NONE',  ( -0.6698729810778066840, -0.09240381056766579226, -2.500000000000000000 ) ) ;
#7323 = CARTESIAN_POINT ( 'NONE',  ( 2.256430356250000102, -3.515624999385482674, -2.763330213280484622E-16 ) ) ;
#7324 =( BOUNDED_CURVE ( )  B_SPLINE_CURVE ( 2, ( #10344, #1693, #20, #6361, #1541, #5379, #8570, #9351, #77 ),
 .UNSPECIFIED., .F., .F. ) 
 B_SPLINE_CURVE_WITH_KNOTS ( ( 3, 2, 2, 2, 3 ),
 ( 0.1875000000000000000, 0.1944444444444444475, 0.2083333333333333426, 0.2222222222222222099, 0.2291666666666666574 ),
 .UNSPECIFIED. ) 
 CURVE ( )  GEOMETRIC_REPRESENTATION_ITEM ( )  RATIONAL_B_SPLINE_CURVE ( ( 0.9330127018922194093, 0.9330127018922194093, 1.000000000000000000, 0.8660254037844387076, 1.000000000000000000, 0.8660254037844387076, 1.000000000000000000, 0.9330127018922194093, 0.9330127018922194093 ) ) 
 REPRESENTATION_ITEM ( '' )  );
#7325 = ADVANCED_FACE ( 'NONE', ( #7617 ), #1298, .T. ) ;
#7326 = CARTESIAN_POINT ( 'NONE',  ( 0.000000000000000000, 0.000000000000000000, 0.000000000000000000 ) ) ;
#7327 = CARTESIAN_POINT ( 'NONE',  ( 1.679787559701184688E-15, 5.283333332240858660, -27.43301270000000258 ) ) ;
#7328 = ADVANCED_FACE ( 'NONE', ( #2130, #9192, #514, #5999, #10203, #1404, #1347, #6782 ), #403, .T. ) ;
#7329 = CARTESIAN_POINT ( 'NONE',  ( 19.09188309203678102, 4.700000000000000178, 19.09188309203678813 ) ) ;
#7330 = CARTESIAN_POINT ( 'NONE',  ( 1.250000000000001110, -3.393749998770965615, 2.165063509461096380 ) ) ;
#7331 = LINE ( 'NONE', #4340, #9624 ) ;
#7332 = CARTESIAN_POINT ( 'NONE',  ( 3.061616997868383141E-16, 0.000000000000000000, 2.500000000000000000 ) ) ;
#7333 = CARTESIAN_POINT ( 'NONE',  ( -20.89169796687544789, 99.50000000000001421, -10.40078880447404330 ) ) ;
#7334 = EDGE_LOOP ( 'NONE', ( #10182, #2699, #6672, #6011 ) ) ;
#7335 = CARTESIAN_POINT ( 'NONE',  ( 3.606694021351891877, 100.0000000000000000, -24.61315535935035115 ) ) ;
#7336 = CARTESIAN_POINT ( 'NONE',  ( 3.701176614148623756, 99.50000000000000000, -24.64875008328975170 ) ) ;
#7337 = CARTESIAN_POINT ( 'NONE',  ( 4.786228327491940187E-16, -4.640624999385481786, 2.605501347177161087 ) ) ;
#7338 = CARTESIAN_POINT ( 'NONE',  ( 2.500000000000000000, -2.418749998770965526, -3.061616997868383141E-16 ) ) ;
#7339 = ADVANCED_FACE ( 'NONE', ( #7732 ), #3599, .F. ) ;
#7340 = CARTESIAN_POINT ( 'NONE',  ( -22.13144646319157260, 99.50000000000001421, -9.428651666388001118 ) ) ;
#7341 = CARTESIAN_POINT ( 'NONE',  ( 4.988497440555089923, 100.0000000000000000, -24.29977663856455194 ) ) ;
#7342 = EDGE_LOOP ( 'NONE', ( #6828, #3468, #1154, #4551 ) ) ;
#7343 = ADVANCED_FACE ( 'NONE', ( #566 ), #10030, .F. ) ;
#7344 = CARTESIAN_POINT ( 'NONE',  ( -2.499999999999999556, -3.956249998770965615, 1.443375672974065882 ) ) ;
#7345 = VERTEX_POINT ( 'NONE', #4485 ) ;
#7346 = DIRECTION ( 'NONE',  ( 0.000000000000000000, 0.000000000000000000, -1.000000000000000000 ) ) ;
#7347 = CARTESIAN_POINT ( 'NONE',  ( 3.446946945638383664, 99.49999999999997158, -21.53774374131874580 ) ) ;
#7348 = CARTESIAN_POINT ( 'NONE',  ( -21.65488089977124275, 99.49999999999997158, -11.10326233039539723 ) ) ;
#7349 = CARTESIAN_POINT ( 'NONE',  ( 1.128215178125001161, -3.590624999385482408, 1.954126010382870815 ) ) ;
#7350 = VERTEX_POINT ( 'NONE', #10147 ) ;
#7351 = CARTESIAN_POINT ( 'NONE',  ( 8.231219904624582639, 99.50000000000000000, 20.21381436664452735 ) ) ;
#7352 = CARTESIAN_POINT ( 'NONE',  ( 0.000000000000000000, 0.000000000000000000, -2.499999999999999556 ) ) ;
#7353 = CARTESIAN_POINT ( 'NONE',  ( -11.18376618407358336, 2.749999997815050445, 26.99999999999999645 ) ) ;
#7354 = CARTESIAN_POINT ( 'NONE',  ( 4.363164797760430424, 99.50000000000002842, -21.67376679147534446 ) ) ;
#7355 = EDGE_CURVE ( 'NONE', #8654, #9400, #7987, .T. ) ;
#7356 = CARTESIAN_POINT ( 'NONE',  ( 3.689266881520847807, 99.99999999999997158, -22.97735580002706968 ) ) ;
#7357 = CARTESIAN_POINT ( 'NONE',  ( 4.320351800798612807, 99.49999999999995737, -21.62386382141117736 ) ) ;
#7358 = CARTESIAN_POINT ( 'NONE',  ( 3.341734429721257005, 99.50000000000000000, -22.34498040423979148 ) ) ;
#7359 = CARTESIAN_POINT ( 'NONE',  ( 27.00000000000000355, 3.849999997815050534, -11.18376618407356737 ) ) ;
#7360 = DIRECTION ( 'NONE',  ( 0.04357787137382919396, -0.9961946980917455452, 0.07547908730517351172 ) ) ;
#7361 = CARTESIAN_POINT ( 'NONE',  ( -21.59424432678268957, 99.49999999999997158, -9.639623801236600897 ) ) ;
#7362 = DIRECTION ( 'NONE',  ( 0.000000000000000000, -1.000000000000000000, 0.000000000000000000 ) ) ;
#7363 = CARTESIAN_POINT ( 'NONE',  ( -21.72555844818415594, 100.0000000000000142, -11.09629251537910655 ) ) ;
#7364 = DIRECTION ( 'NONE',  ( 0.000000000000000000, 0.000000000000000000, -1.000000000000000000 ) ) ;
#7365 = ORIENTED_EDGE ( 'NONE', *, *, #5652, .T. ) ;
#7366 = ADVANCED_BREP_SHAPE_REPRESENTATION ( '', ( #6298, #5055 ), #5746 ) ;
#7367 = CARTESIAN_POINT ( 'NONE',  ( 1.128215178125001161, -3.590624999385482408, 1.954126010382870815 ) ) ;
#7368 = DIRECTION ( 'NONE',  ( 1.000000000000000000, 0.000000000000000000, 0.000000000000000000 ) ) ;
#7369 = CARTESIAN_POINT ( 'NONE',  ( -2.500000000000000000, -2.737499999999999822, -1.443375672974064106 ) ) ;
#7370 = LINE ( 'NONE', #9878, #6388 ) ;
#7371 = CARTESIAN_POINT ( 'NONE',  ( -5.039362679103552881E-15, 3.249999998907525001, 27.43301270000000258 ) ) ;
#7372 = CARTESIAN_POINT ( 'NONE',  ( -20.61566945723384592, 100.0000000000000000, -10.83949095114527594 ) ) ;
#7373 = AXIS2_PLACEMENT_3D ( 'NONE', #2241, #5998, #4533 ) ;
#7374 = LINE ( 'NONE', #8269, #3776 ) ;
#7375 = DIRECTION ( 'NONE',  ( -0.8799640205556051864, 0.000000000000000000, -0.4750403377899757862 ) ) ;
#7376 = CARTESIAN_POINT ( 'NONE',  ( 0.000000000000000000, 0.000000000000000000, -25.15000000000000213 ) ) ;
#7377 = ORIENTED_EDGE ( 'NONE', *, *, #3276, .T. ) ;
#7378 = ORIENTED_EDGE ( 'NONE', *, *, #3637, .F. ) ;
#7379 =( BOUNDED_CURVE ( )  B_SPLINE_CURVE ( 2, ( #4361, #1120, #3640, #4261, #9177, #7547, #5984, #1225, #1893 ),
 .UNSPECIFIED., .F., .T. ) 
 B_SPLINE_CURVE_WITH_KNOTS ( ( 3, 2, 2, 2, 3 ),
 ( 0.4642857142857143016, 0.4821428571428571508, 0.5000000000000000000, 0.5178571428571429047, 0.5357142857142856984 ),
 .UNSPECIFIED. ) 
 CURVE ( )  GEOMETRIC_REPRESENTATION_ITEM ( )  RATIONAL_B_SPLINE_CURVE ( ( 1.000000000000000000, 0.9238795325112867385, 1.000000000000000000, 0.9238795325112867385, 1.000000000000000000, 0.9238795325112867385, 1.000000000000000000, 0.9238795325112867385, 1.000000000000000000 ) ) 
 REPRESENTATION_ITEM ( '' )  );
#7380 = CARTESIAN_POINT ( 'NONE',  ( -21.59614764830937972, 99.99999999999994316, -9.292069227195950631 ) ) ;
#7381 = CARTESIAN_POINT ( 'NONE',  ( 19.39806930854668110, 4.349999998907525089, -19.39806930854668110 ) ) ;
#7382 = CARTESIAN_POINT ( 'NONE',  ( -16.30857500771091040, 99.49999999999994316, 15.34700649443169063 ) ) ;
#7383 = DIRECTION ( 'NONE',  ( -0.000000000000000000, 1.000000000000000000, -0.000000000000000000 ) ) ;
#7384 = CARTESIAN_POINT ( 'NONE',  ( 4.996790860652426159E-15, -2.306249998770965259, -2.500000000000000000 ) ) ;
#7385 = CARTESIAN_POINT ( 'NONE',  ( -16.60513711880302878, 100.0000000000000000, 15.15667007515659570 ) ) ;
#7386 = CARTESIAN_POINT ( 'NONE',  ( 4.503533123526070270, 99.99999999999995737, -24.63026223303895890 ) ) ;
#7387 = AXIS2_PLACEMENT_3D ( 'NONE', #1103, #270, #7531 ) ;
#7388 = CARTESIAN_POINT ( 'NONE',  ( 2.500000000000000000, -4.181249998770965703, -1.443375672974064994 ) ) ;
#7389 = EDGE_LOOP ( 'NONE', ( #5434, #7943, #9288, #2481 ) ) ;
#7390 = EDGE_CURVE ( 'NONE', #8910, #3336, #1651, .T. ) ;
#7391 = CARTESIAN_POINT ( 'NONE',  ( 0.000000000000000000, 85.00000000000000000, 0.000000000000000000 ) ) ;
#7392 = CARTESIAN_POINT ( 'NONE',  ( 3.446946945638383664, 99.99999999999994316, -21.53774374131874580 ) ) ;
#7393 = CARTESIAN_POINT ( 'NONE',  ( -14.97579057656165169, 100.0000000000000142, 16.56690896377573452 ) ) ;
#7394 = CARTESIAN_POINT ( 'NONE',  ( 4.772556553149396308, 99.49999999999997158, -24.49721679606612312 ) ) ;
#7395 = VECTOR ( 'NONE', #589, 1000.000000000000000 ) ;
#7396 = CARTESIAN_POINT ( 'NONE',  ( -15.30066472929571653, 99.49999999999998579, 16.41738810589640707 ) ) ;
#7397 = DIRECTION ( 'NONE',  ( 0.000000000000000000, 1.000000000000000000, 0.000000000000000000 ) ) ;
#7398 = DIRECTION ( 'NONE',  ( -0.000000000000000000, -1.000000000000000000, -0.000000000000000000 ) ) ;
#7399 = VERTEX_POINT ( 'NONE', #9471 ) ;
#7400 = CARTESIAN_POINT ( 'NONE',  ( 3.080354370726382296, 100.0000000000000426, -23.09295995363041598 ) ) ;
#7401 = LINE ( 'NONE', #9137, #204 ) ;
#7402 = CARTESIAN_POINT ( 'NONE',  ( 3.504547665631520648, 99.99999999999994316, -23.10026541809159184 ) ) ;
#7403 = CARTESIAN_POINT ( 'NONE',  ( 8.393217272293057363, 99.50000000000000000, 19.69436072183531650 ) ) ;
#7404 = DIRECTION ( 'NONE',  ( 0.000000000000000000, -1.000000000000000000, 0.000000000000000000 ) ) ;
#7405 = CARTESIAN_POINT ( 'NONE',  ( 11.18376618407356915, 4.749999997815050001, -27.00000000000000355 ) ) ;
#7406 = EDGE_CURVE ( 'NONE', #8654, #1114, #4651, .T. ) ;
#7407 = LINE ( 'NONE', #8895, #5010 ) ;
#7408 = CARTESIAN_POINT ( 'NONE',  ( -21.13452028402337035, 100.0000000000000000, -9.824917503107416294 ) ) ;
#7409 =( NAMED_UNIT ( * ) PLANE_ANGLE_UNIT ( ) SI_UNIT ( $, .RADIAN. ) );
#7410 = EDGE_CURVE ( 'NONE', #393, #6584, #6373, .T. ) ;
#7411 = FACE_OUTER_BOUND ( 'NONE', #10310, .T. ) ;
#7412 = DIRECTION ( 'NONE',  ( 0.05468478504300072068, 0.000000000000000000, 0.9985036676371302766 ) ) ;
#7413 = DIRECTION ( 'NONE',  ( -0.000000000000000000, -1.000000000000000000, -0.000000000000000000 ) ) ;
#7414 = ORIENTED_EDGE ( 'NONE', *, *, #1752, .T. ) ;
#7415 = ORIENTED_EDGE ( 'NONE', *, *, #6350, .T. ) ;
#7416 = CARTESIAN_POINT ( 'NONE',  ( -1.595409442497313560E-16, -4.753124999385481608, -2.605501347177161087 ) ) ;
#7417 = PRESENTATION_STYLE_ASSIGNMENT (( #257 ) ) ;
#7418 = CARTESIAN_POINT ( 'NONE',  ( -15.03963071504896121, 99.50000000000001421, 16.63526396357264758 ) ) ;
#7419 = CARTESIAN_POINT ( 'NONE',  ( 1.128215178124999607, -0.4031249993854829627, -1.954126010382871259 ) ) ;
#7420 = CARTESIAN_POINT ( 'NONE',  ( 1.679787559701184688E-15, 2.049999998907525711, -27.43301270000000258 ) ) ;
#7421 = CARTESIAN_POINT ( 'NONE',  ( -4.959819536546781389E-15, 1.399999999999999911, 27.00000000000000355 ) ) ;
#7422 = DIRECTION ( 'NONE',  ( 0.000000000000000000, 0.000000000000000000, -1.000000000000000000 ) ) ;
#7423 = CARTESIAN_POINT ( 'NONE',  ( 4.723706824522782455, 100.0000000000000000, -24.08630974238606370 ) ) ;
#7424 = CARTESIAN_POINT ( 'NONE',  ( 8.133363296361027395, 100.0000000000000426, 19.85287606700953233 ) ) ;
#7425 = VERTEX_POINT ( 'NONE', #7894 ) ;
#7426 = CARTESIAN_POINT ( 'NONE',  ( 7.812290123947159159, 99.49999999999998579, 21.17203503082402349 ) ) ;
#7427 = FACE_OUTER_BOUND ( 'NONE', #691, .T. ) ;
#7428 = CYLINDRICAL_SURFACE ( 'NONE', #7387, 2.500000000000000000 ) ;
#7429 =( LENGTH_UNIT ( ) NAMED_UNIT ( * ) SI_UNIT ( .MILLI., .METRE. ) );
#7430 = CARTESIAN_POINT ( 'NONE',  ( -1.128215178124998497, -5.128124999385482496, 1.954126010382872147 ) ) ;
#7431 = CARTESIAN_POINT ( 'NONE',  ( 8.901217755223779449, 99.50000000000004263, 19.92336871027421097 ) ) ;
#7432 = CARTESIAN_POINT ( 'NONE',  ( 3.764204346677844093, 99.50000000000001421, -22.52576385118515745 ) ) ;
#7433 = LINE ( 'NONE', #4458, #5093 ) ;
#7434 =( BOUNDED_CURVE ( )  B_SPLINE_CURVE ( 2, ( #9206, #10221, #635, #2206, #689, #3779, #8652, #586, #477, #2263, #5289, #6070, #1364, #5408, #9261, #6909, #8601, #2152, #6966, #1474, #2094, #1314, #3052, #6017, #4558, #534, #6180, #6234, #7755, #9378, #10167, #3004, #1424, #3673, #7697, #5229, #4612, #5462, #9435, #9320, #7016, #5351, #7806, #2034, #4450, #6853, #8429, #3727, #3834, #10107, #1261, #2943, #4669, #6125, #10049, #8485, #7860, #7637, #2886, #4504, #8541, #3881, #7069, #2834, #5559, #1726, #4821, #2468, #8703, #3, #1628, #3937, #7122, #10325, #8017, #3302, #5513, #9633, #9583, #5663, #3160, #1680, #1524, #8852, #4873, #2414, #8063, #6343, #848, #4766, #2313, #897, #4140, #8115, #55, #5713, #4717, #7963, #7910, #799, #6442, #4086, #8751, #7271, #1575, #743, #110, #946, #9538, #2362, #3990, #3206, #7175, #4918, #4038, #6491, #6390, #5610, #7221, #8799, #3254, #9490, #9682, #2522, #8900, #10275, #3109, #6291, #5008, #9098, #8946, #2713, #1916, #9826, #5902 ),
 .UNSPECIFIED., .F., .F. ) 
 B_SPLINE_CURVE_WITH_KNOTS ( ( 3, 2, 2, 2, 2, 2, 2, 2, 2, 2, 2, 2, 2, 2, 2, 2, 2, 2, 2, 2, 2, 2, 2, 2, 2, 2, 2, 2, 2, 2, 2, 2, 2, 2, 2, 2, 2, 2, 2, 2, 2, 2, 2, 2, 2, 2, 2, 2, 2, 2, 2, 2, 2, 2, 2, 2, 2, 2, 2, 2, 2, 2, 2, 2, 2, 2, 2, 3 ),
 ( 0.000000000000000000, 0.01500076742380700850, 0.03000153484761401701, 0.04500230227142102551, 0.06000306969522803402, 0.07500383711903504946, 0.09000460454284205103, 0.1050053719666490665, 0.1200061393904560680, 0.1350069068142630835, 0.1500076742380700989, 0.1650084416618771144, 0.1800092090856841021, 0.1950099765094911175, 0.2100107439332981329, 0.2250115113571051484, 0.2400122787809121361, 0.2550130462047191515, 0.2700138136285261670, 0.2850145810523331824, 0.3000153484761401979, 0.3150161158999472133, 0.3300168833237542287, 0.3450176507475611887, 0.3600184181713682041, 0.3750191855951752196, 0.3900199530189822350, 0.4050207204427892504, 0.4200214878665962659, 0.4350222552904032813, 0.4500230227142102968, 0.4650237901380173122, 0.4800245575618242722, 0.4950253249856312876, 0.5100260924094383030, 0.5250268598332453740, 0.5400276272570523339, 0.5550283946808592939, 0.5700291621046663648, 0.5850299295284733248, 0.6000306969522803957, 0.6150314643760873556, 0.6300322317998944266, 0.6450329992237013865, 0.6600337666475084575, 0.6750345340713154174, 0.6900353014951223773, 0.7050360689189294483, 0.7200368363427364082, 0.7350376037665434792, 0.7500383711903504391, 0.7650391386141575101, 0.7800399060379644700, 0.7950406734617715410, 0.8100414408855785009, 0.8250422083093854608, 0.8400429757331925318, 0.8550437431569994917, 0.8700445105808065627, 0.8850452780046135226, 0.9000460454284205936, 0.9150468128522275535, 0.9300475802760346244, 0.9450483476998415844, 0.9600491151236485443, 0.9750498825474556153, 0.9900506499712625752, 1.000000000000000000 ),
 .UNSPECIFIED. ) 
 CURVE ( )  GEOMETRIC_REPRESENTATION_ITEM ( )  RATIONAL_B_SPLINE_CURVE ( ( 1.000000000000000000, 0.8660254037844387076, 1.000000000000000000, 0.8660254037844387076, 1.000000000000000000, 0.8660254037844387076, 1.000000000000000000, 0.8660254037844387076, 1.000000000000000000, 0.8660254037844387076, 1.000000000000000000, 0.8660254037844387076, 1.000000000000000000, 0.8660254037844387076, 1.000000000000000000, 0.8660254037844387076, 1.000000000000000000, 0.8660254037844387076, 1.000000000000000000, 0.8660254037844387076, 1.000000000000000000, 0.8660254037844387076, 1.000000000000000000, 0.8660254037844387076, 1.000000000000000000, 0.8660254037844387076, 1.000000000000000000, 0.8660254037844387076, 1.000000000000000000, 0.8660254037844387076, 1.000000000000000000, 0.8660254037844387076, 1.000000000000000000, 0.8660254037844387076, 1.000000000000000000, 0.8660254037844387076, 1.000000000000000000, 0.8660254037844387076, 1.000000000000000000, 0.8660254037844387076, 1.000000000000000000, 0.8660254037844387076, 1.000000000000000000, 0.8660254037844387076, 1.000000000000000000, 0.8660254037844387076, 1.000000000000000000, 0.8660254037844387076, 1.000000000000000000, 0.8660254037844387076, 1.000000000000000000, 0.8660254037844387076, 1.000000000000000000, 0.8660254037844387076, 1.000000000000000000, 0.8660254037844387076, 1.000000000000000000, 0.8660254037844387076, 1.000000000000000000, 0.8660254037844387076, 1.000000000000000000, 0.8660254037844387076, 1.000000000000000000, 0.8660254037844387076, 1.000000000000000000, 0.8660254037844387076, 1.000000000000000000, 0.8660254037844387076, 1.000000000000000000, 0.8660254037844387076, 1.000000000000000000, 0.8660254037844387076, 1.000000000000000000, 0.8660254037844387076, 1.000000000000000000, 0.8660254037844387076, 1.000000000000000000, 0.8660254037844387076, 1.000000000000000000, 0.8660254037844387076, 1.000000000000000000, 0.8660254037844387076, 1.000000000000000000, 0.8660254037844387076, 1.000000000000000000, 0.8660254037844387076, 1.000000000000000000, 0.8660254037844387076, 1.000000000000000000, 0.8660254037844387076, 1.000000000000000000, 0.8660254037844387076, 1.000000000000000000, 0.8660254037844387076, 1.000000000000000000, 0.8660254037844387076, 1.000000000000000000, 0.8660254037844387076, 1.000000000000000000, 0.8660254037844387076, 1.000000000000000000, 0.8660254037844387076, 1.000000000000000000, 0.8660254037844387076, 1.000000000000000000, 0.8660254037844387076, 1.000000000000000000, 0.8660254037844387076, 1.000000000000000000, 0.8660254037844387076, 1.000000000000000000, 0.8660254037844387076, 1.000000000000000000, 0.8660254037844387076, 1.000000000000000000, 0.8660254037844387076, 1.000000000000000000, 0.8660254037844387076, 1.000000000000000000, 0.8660254037844387076, 1.000000000000000000, 0.8660254037844387076, 1.000000000000000000, 0.8660254037844387076, 1.000000000000000000, 0.8660254037844387076, 1.000000000000000000, 0.8660254037844387076, 1.000000000000000000, 0.8660254037844387076, 1.000000000000000000, 0.8660254037844387076, 1.000000000000000000, 0.9111405360107182050, 0.9401542295229976531 ) ) 
 REPRESENTATION_ITEM ( '' )  );
#7435 = CARTESIAN_POINT ( 'NONE',  ( 2.256430356250000546, -0.5156249993854828961, 1.302750673588579877 ) ) ;
#7436 = ORIENTED_EDGE ( 'NONE', *, *, #9968, .F. ) ;
#7437 = VERTEX_POINT ( 'NONE', #8835 ) ;
#7438 = CARTESIAN_POINT ( 'NONE',  ( -22.55793349878803156, 100.0000000000000000, -10.88926985104519929 ) ) ;
#7439 = CARTESIAN_POINT ( 'NONE',  ( 3.198592217420132666, 99.50000000000000000, -21.96964977087737836 ) ) ;
#7440 = LINE ( 'NONE', #7659, #6875 ) ;
#7441 = DIRECTION ( 'NONE',  ( 0.000000000000000000, 0.000000000000000000, -1.000000000000000000 ) ) ;
#7442 = ADVANCED_FACE ( 'NONE', ( #6427 ), #726, .F. ) ;
#7443 = CARTESIAN_POINT ( 'NONE',  ( 4.996790860652426159E-15, -1.462499999999999911, -2.500000000000000000 ) ) ;
#7444 = VECTOR ( 'NONE', #4930, 1000.000000000000000 ) ;
#7445 = PLANE ( 'NONE',  #4311 ) ;
#7446 = CARTESIAN_POINT ( 'NONE',  ( 4.232798786556307036, 99.50000000000000000, -24.34936571594186105 ) ) ;
#7447 = CARTESIAN_POINT ( 'NONE',  ( 4.835062408351179286, 99.50000000000000000, -21.79588013901878440 ) ) ;
#7448 = VERTEX_POINT ( 'NONE', #7949 ) ;
#7449 = VECTOR ( 'NONE', #7413, 1000.000000000000000 ) ;
#7450 = CARTESIAN_POINT ( 'NONE',  ( 21.47055288461538325, 99.50000000000000000, -0.7081330128205128860 ) ) ;
#7451 = CARTESIAN_POINT ( 'NONE',  ( 27.43301269999999548, 4.299999998907526155, 11.36312591709337738 ) ) ;
#7452 = CARTESIAN_POINT ( 'NONE',  ( -7.500000000000000000, 105.0000000000000142, -0.9999999999999997780 ) ) ;
#7453 = APPLICATION_CONTEXT ( 'automotive_design' ) ;
#7454 = TOROIDAL_SURFACE ( 'NONE', #1774, 23.82500000000000284, 1.324999999999999956 ) ;
#7455 = CARTESIAN_POINT ( 'NONE',  ( 3.306546357697854128E-15, 100.0000000000000000, 27.00000000000000355 ) ) ;
#7456 = CARTESIAN_POINT ( 'NONE',  ( 7.856939908706818798, 99.99999999999995737, 20.19612520319305560 ) ) ;
#7457 = EDGE_CURVE ( 'NONE', #4244, #10122, #3141, .T. ) ;
#7458 = ORIENTED_EDGE ( 'NONE', *, *, #2041, .F. ) ;
#7459 = CARTESIAN_POINT ( 'NONE',  ( 3.659868213429061878, 100.0000000000000284, -22.50687739797974274 ) ) ;
#7460 = CARTESIAN_POINT ( 'NONE',  ( -11.18376618407358336, 2.749999997815050445, 26.99999999999999645 ) ) ;
#7461 = CARTESIAN_POINT ( 'NONE',  ( 5.725936192474917696, 99.50000000000000000, 21.08018326417248645 ) ) ;
#7462 = CYLINDRICAL_SURFACE ( 'NONE', #6988, 7.500000000000000000 ) ;
#7463 = CARTESIAN_POINT ( 'NONE',  ( -21.86704275050744073, 100.0000000000000142, -11.06111336656620026 ) ) ;
#7464 = CARTESIAN_POINT ( 'NONE',  ( 2.955068081869620666, 99.99999999999998579, -21.57801138750623338 ) ) ;
#7465 =( GEOMETRIC_REPRESENTATION_CONTEXT ( 3 ) GLOBAL_UNCERTAINTY_ASSIGNED_CONTEXT ( ( #4760 ) ) GLOBAL_UNIT_ASSIGNED_CONTEXT ( ( #6296, #6240, #8022 ) ) REPRESENTATION_CONTEXT ( 'NONE', 'WORKASPACE' ) );
#7466 = CARTESIAN_POINT ( 'NONE',  ( 0.6698729810778112359, -4.632596189432333311, -2.499999999999996447 ) ) ;
#7467 = CARTESIAN_POINT ( 'NONE',  ( 1.250000000000001110, -0.2999999999999999889, 2.165063509461096380 ) ) ;
#7468 = EDGE_CURVE ( 'NONE', #3208, #3431, #2114, .T. ) ;
#7469 = CARTESIAN_POINT ( 'NONE',  ( -14.83571502646304197, 99.50000000000004263, 16.32397075880403392 ) ) ;
#7470 = DIRECTION ( 'NONE',  ( 0.000000000000000000, 0.000000000000000000, -1.000000000000000000 ) ) ;
#7471 = CARTESIAN_POINT ( 'NONE',  ( -27.43301270000000969, 1.499999998907525445, 11.36312591709335429 ) ) ;
#7472 = EDGE_CURVE ( 'NONE', #5726, #2184, #8068, .T. ) ;
#7473 = CARTESIAN_POINT ( 'NONE',  ( -20.42657152723830905, 99.99999999999997158, -10.54129411626120216 ) ) ;
#7474 = FACE_OUTER_BOUND ( 'NONE', #677, .T. ) ;
#7475 = CIRCLE ( 'NONE', #2987, 23.99999999999999645 ) ;
#7476 = CARTESIAN_POINT ( 'NONE',  ( 9.820792995160308791, 100.0000000000000000, 20.21220011423140761 ) ) ;
#7477 = DIRECTION ( 'NONE',  ( -1.000000000000000000, 0.000000000000000000, 0.000000000000000000 ) ) ;
#7478 = EDGE_CURVE ( 'NONE', #4703, #1808, #3328, .T. ) ;
#7479 = CARTESIAN_POINT ( 'NONE',  ( -21.03505001771060634, 99.99999999999994316, -9.476849197711761263 ) ) ;
#7480 = CARTESIAN_POINT ( 'NONE',  ( 3.409892249890944527, 100.0000000000000000, -24.50637943905448779 ) ) ;
#7481 =( NAMED_UNIT ( * ) SI_UNIT ( $, .STERADIAN. ) SOLID_ANGLE_UNIT ( ) );
#7482 = VECTOR ( 'NONE', #9913, 1000.000000000000000 ) ;
#7483 = CARTESIAN_POINT ( 'NONE',  ( -1.728529299398585906, -5.253648441416169490, -1.450401466387756244 ) ) ;
#7484 = DIRECTION ( 'NONE',  ( -0.000000000000000000, -1.000000000000000000, -0.000000000000000000 ) ) ;
#7485 = EDGE_CURVE ( 'NONE', #4596, #8813, #6522, .T. ) ;
#7486 = CARTESIAN_POINT ( 'NONE',  ( 9.554054106072296548, 99.50000000000001421, 20.45778517829714360 ) ) ;
#7487 = CARTESIAN_POINT ( 'NONE',  ( -21.59424432678268957, 99.99999999999997158, -9.639623801236600897 ) ) ;
#7488 = VERTEX_POINT ( 'NONE', #1020 ) ;
#7489 = DIRECTION ( 'NONE',  ( -0.000000000000000000, 1.000000000000000000, -0.000000000000000000 ) ) ;
#7490 = CARTESIAN_POINT ( 'NONE',  ( -1.128215178125000273, -1.228124999385483029, -1.954126010382871259 ) ) ;
#7491 = ORIENTED_EDGE ( 'NONE', *, *, #1160, .T. ) ;
#7492 = CARTESIAN_POINT ( 'NONE',  ( 6.123233995736727825E-17, -25.00000000000000000, 0.4999999999999968914 ) ) ;
#7493 = CARTESIAN_POINT ( 'NONE',  ( 3.497829868842083023, 99.50000000000000000, -21.50512556757917793 ) ) ;
#7494 = CARTESIAN_POINT ( 'NONE',  ( 3.277744210708366079, 99.50000000000001421, -23.71256836663369327 ) ) ;
#7495 = DIRECTION ( 'NONE',  ( 0.000000000000000000, 0.000000000000000000, -1.000000000000000000 ) ) ;
#7497 = ADVANCED_FACE ( 'NONE', ( #8241 ), #979, .T. ) ;
#7496 = CARTESIAN_POINT ( 'NONE',  ( -15.27171031718473770, 99.50000000000002842, 15.44886715306589764 ) ) ;
#7498 = CARTESIAN_POINT ( 'NONE',  ( 0.000000000000000000, 0.000000000000000000, 0.000000000000000000 ) ) ;
#7499 = PLANE ( 'NONE',  #7623 ) ;
#7500 = CARTESIAN_POINT ( 'NONE',  ( 9.468852706215191262, 100.0000000000000000, 21.22967007823213237 ) ) ;
#7501 = EDGE_LOOP ( 'NONE', ( #2121, #2075, #9108, #5475 ) ) ;
#7502 = B_SPLINE_CURVE_WITH_KNOTS ( 'NONE', 3,
 ( #6018, #1315, #2095, #8376, #6910, #371, #2944, #2887, #7529, #3674, #3507 ),
 .UNSPECIFIED., .F., .F.,
 ( 4, 1, 1, 1, 1, 1, 1, 1, 4 ),
 ( 0.000000000000000000, 0.1243175037779491315, 0.2437391319546453605, 0.3610119291759345539, 0.4796059399169178006, 0.5994854737745749507, 0.7252340722053824962, 0.8585022233306516259, 1.000000000000000000 ),
 .UNSPECIFIED. ) ;
#7503 = CARTESIAN_POINT ( 'NONE',  ( 0.000000000000000000, 5.000000000000000000, 0.000000000000000000 ) ) ;
#7504 = CARTESIAN_POINT ( 'NONE',  ( -27.43301270000000969, 2.399999998907525356, 11.36312591709335429 ) ) ;
#7505 = CARTESIAN_POINT ( 'NONE',  ( 3.739209042966563867, 99.50000000000000000, -21.42288334414699236 ) ) ;
#7506 = CARTESIAN_POINT ( 'NONE',  ( 3.538198506519217190, 99.49999999999998579, -24.58220198924426114 ) ) ;
#7507 = CARTESIAN_POINT ( 'NONE',  ( 7.913184448816831029, 99.99999999999994316, 20.09878816755126252 ) ) ;
#7508 = ORIENTED_EDGE ( 'NONE', *, *, #7390, .F. ) ;
#7509 = CARTESIAN_POINT ( 'NONE',  ( 3.028692941384139026, 99.50000000000001421, -22.52214499033115302 ) ) ;
#7510 = CARTESIAN_POINT ( 'NONE',  ( -27.00000000000001421, 5.049999997815051600, 11.18376618407356382 ) ) ;
#7511 = CARTESIAN_POINT ( 'NONE',  ( -3.000000000000000888, -15.00000000000000000, -1.732050807568877415 ) ) ;
#7512 = CARTESIAN_POINT ( 'NONE',  ( -21.73488407773357167, 99.50000000000000000, -9.647150398373231184 ) ) ;
#7513 = DIRECTION ( 'NONE',  ( 0.000000000000000000, 0.000000000000000000, 1.000000000000000000 ) ) ;
#7514 = CARTESIAN_POINT ( 'NONE',  ( -22.20893716642541804, 99.50000000000002842, -10.81429252070940272 ) ) ;
#7515 = CARTESIAN_POINT ( 'NONE',  ( 3.428579745388047328, 99.99999999999998579, -21.16399209792802694 ) ) ;
#7516 = CARTESIAN_POINT ( 'NONE',  ( -4.357666448243394824E-15, -2.137500000000000178, 2.500000000000000000 ) ) ;
#7517 = EDGE_CURVE ( 'NONE', #600, #8002, #1138, .T. ) ;
#7518 = CARTESIAN_POINT ( 'NONE',  ( -2.499999999999999556, -1.762499999999999734, 1.443375672974065882 ) ) ;
#7519 = SHAPE_DEFINITION_REPRESENTATION ( #846, #1584 ) ;
#7520 = CARTESIAN_POINT ( 'NONE',  ( -4.357666448243394824E-15, -2.587499999999999467, 2.500000000000000000 ) ) ;
#7521 = CARTESIAN_POINT ( 'NONE',  ( 2.924645347134957163, 100.0000000000000142, -23.60918035669702064 ) ) ;
#7522 = CARTESIAN_POINT ( 'NONE',  ( -27.43301270000000258, 2.249999998907525001, -3.359575119402369376E-15 ) ) ;
#7523 = CARTESIAN_POINT ( 'NONE',  ( 0.000000000000000000, 85.00000000000000000, 0.000000000000000000 ) ) ;
#7524 = CARTESIAN_POINT ( 'NONE',  ( 0.000000000000000000, 105.0000000000000142, 0.000000000000000000 ) ) ;
#7525 = CARTESIAN_POINT ( 'NONE',  ( 7.156925775808251622, 100.0000000000000000, 23.91622092442889524 ) ) ;
#7526 = DIRECTION ( 'NONE',  ( 0.000000000000000000, 0.000000000000000000, -1.000000000000000000 ) ) ;
#7527 = EDGE_LOOP ( 'NONE', ( #5082, #909, #8173, #8979 ) ) ;
#7528 = DIRECTION ( 'NONE',  ( -0.9567206510497618943, 0.000000000000000000, 0.2910078965507976179 ) ) ;
#7529 = CARTESIAN_POINT ( 'NONE',  ( 3.298672054714395063, 100.0000000000000142, -22.72039518595936869 ) ) ;
#7530 = CARTESIAN_POINT ( 'NONE',  ( -2.256430356249999214, -0.5531249993854828739, 1.302750673588581876 ) ) ;
#7531 = DIRECTION ( 'NONE',  ( 0.000000000000000000, 0.000000000000000000, -1.000000000000000000 ) ) ;
#7532 = SURFACE_STYLE_USAGE ( .BOTH. , #8177 ) ;
#7533 = CARTESIAN_POINT ( 'NONE',  ( -2.500000000000000000, -1.781249998770965570, -1.443375672974064106 ) ) ;
#7534 = VECTOR ( 'NONE', #2340, 1000.000000000000000 ) ;
#7535 = CARTESIAN_POINT ( 'NONE',  ( 3.873456569393397331, 99.50000000000002842, -22.53291374702356364 ) ) ;
#7536 = CARTESIAN_POINT ( 'NONE',  ( -21.94169572595625795, 100.0000000000000000, -9.715372641902229489 ) ) ;
#7537 = ORIENTED_EDGE ( 'NONE', *, *, #7111, .F. ) ;
#7538 = DIRECTION ( 'NONE',  ( 0.000000000000000000, 0.000000000000000000, -1.000000000000000000 ) ) ;
#7539 = EDGE_CURVE ( 'NONE', #9964, #4732, #4171, .T. ) ;
#7540 = CARTESIAN_POINT ( 'NONE',  ( -1.128215178124998497, -1.078124999385482674, 1.954126010382872147 ) ) ;
#7541 = VERTEX_POINT ( 'NONE', #338 ) ;
#7542 = CIRCLE ( 'NONE', #3059, 18.23673019291534558 ) ;
#7543 = EDGE_CURVE ( 'NONE', #8002, #7847, #9759, .T. ) ;
#7544 = LINE ( 'NONE', #6761, #8651 ) ;
#7545 = CARTESIAN_POINT ( 'NONE',  ( 3.739209042966563867, 99.99999999999997158, -21.42288334414699236 ) ) ;
#7546 = DIRECTION ( 'NONE',  ( -2.406779422944247204E-17, 0.9949358851208914833, 0.1005116137503925117 ) ) ;
#7547 = CARTESIAN_POINT ( 'NONE',  ( -27.00000000000001421, 3.449999997815051067, 11.18376618407356560 ) ) ;
#7548 = AXIS2_PLACEMENT_3D ( 'NONE', #4221, #8349, #9086 ) ;
#7549 = B_SPLINE_CURVE_WITH_KNOTS ( 'NONE', 3,
 ( #4202, #133, #8971, #7386, #4983, #3227, #6466, #2437, #2491, #7341, #4112, #6605, #870, #8182, #965, #1011, #225, #1697, #5632 ),
 .UNSPECIFIED., .F., .F.,
 ( 4, 1, 1, 1, 1, 1, 1, 1, 1, 1, 1, 1, 1, 1, 1, 1, 4 ),
 ( 0.000000000000000000, 0.06533929434940796699, 0.1284421010879715219, 0.1894557237235162950, 0.2487158350925330053, 0.3070727012892665031, 0.3650088636856013702, 0.4229902474982629723, 0.4815891416229265420, 0.5404453987529589387, 0.6002338948610608238, 0.6608164219703346332, 0.7232441343194829786, 0.7881366429682739039, 0.8556965829275263724, 0.9259544997225339635, 1.000000000000000000 ),
 .UNSPECIFIED. ) ;
#7550 = CARTESIAN_POINT ( 'NONE',  ( -15.13293277027690209, 99.50000000000000000, 16.13104881108577970 ) ) ;
#7551 = CARTESIAN_POINT ( 'NONE',  ( 9.676361905416721143, 99.50000000000001421, 21.63547735782115566 ) ) ;
#7552 = LINE ( 'NONE', #772, #4292 ) ;
#7553 = CARTESIAN_POINT ( 'NONE',  ( 9.342627931057743140, 100.0000000000000000, 21.59831790269294771 ) ) ;
#7554 = AXIS2_PLACEMENT_3D ( 'NONE', #4432, #352, #1035 ) ;
#7555 = VERTEX_POINT ( 'NONE', #7352 ) ;
#7556 = CARTESIAN_POINT ( 'NONE',  ( 19.09188309203678813, 1.499999997815050223, -19.09188309203678813 ) ) ;
#7557 = CARTESIAN_POINT ( 'NONE',  ( 27.43301270000000258, 4.399999998907525800, -11.36312591709336139 ) ) ;
#7558 = DIRECTION ( 'NONE',  ( 0.7071067811865473507, 0.000000000000000000, 0.7071067811865477948 ) ) ;
#7559 = CARTESIAN_POINT ( 'NONE',  ( 9.861577898019769250, 99.49999999999995737, 21.03794551367759169 ) ) ;
#7560 = CARTESIAN_POINT ( 'NONE',  ( 11.18376618407357093, 4.749999997815051778, -27.00000000000000355 ) ) ;
#7561 = VERTEX_POINT ( 'NONE', #4124 ) ;
#7562 = LINE ( 'NONE', #3596, #4602 ) ;
#7563 = CARTESIAN_POINT ( 'NONE',  ( 26.99999999999999645, 3.749999997815050445, 11.18376618407358691 ) ) ;
#7564 = SURFACE_SIDE_STYLE ('',( #7675 ) ) ;
#7565 =( GEOMETRIC_REPRESENTATION_CONTEXT ( 3 ) GLOBAL_UNCERTAINTY_ASSIGNED_CONTEXT ( ( #3720 ) ) GLOBAL_UNIT_ASSIGNED_CONTEXT ( ( #9441, #3887, #6397 ) ) REPRESENTATION_CONTEXT ( 'NONE', 'WORKASPACE' ) );
#7566 = DIRECTION ( 'NONE',  ( 0.000000000000000000, 0.000000000000000000, -1.000000000000000000 ) ) ;
#7567 = FILL_AREA_STYLE_COLOUR ( '', #5220 ) ;
#7568 = EDGE_LOOP ( 'NONE', ( #10365, #7923, #770, #721, #2973, #7995 ) ) ;
#7569 = CARTESIAN_POINT ( 'NONE',  ( 4.887668416326221177, 100.0000000000000142, -23.70513093767710089 ) ) ;
#7570 = CARTESIAN_POINT ( 'NONE',  ( 27.43301270000000258, 0.3999999989075253559, -11.36312591709336139 ) ) ;
#7571 = VERTEX_POINT ( 'NONE', #7307 ) ;
#7572 = CARTESIAN_POINT ( 'NONE',  ( 2.500000000000000444, -1.612499999999999822, 1.443375672974063439 ) ) ;
#7573 = SHAPE_DEFINITION_REPRESENTATION ( #8867, #9736 ) ;
#7574 = CARTESIAN_POINT ( 'NONE',  ( -14.89910828679519739, 99.49999999999997158, 16.44921749203638939 ) ) ;
#7575 = CARTESIAN_POINT ( 'NONE',  ( 1.128215178125001161, -0.5531249993854828739, 1.954126010382870815 ) ) ;
#7576 = CARTESIAN_POINT ( 'NONE',  ( 11.36312591709336850, 1.699999998907525400, 27.43301269999999903 ) ) ;
#7577 = CARTESIAN_POINT ( 'NONE',  ( -0.6698729810778069060, -0.9924038105676656896, -2.500000000000000000 ) ) ;
#7578 = EDGE_LOOP ( 'NONE', ( #9923, #598, #4843, #6124 ) ) ;
#7579 = EDGE_CURVE ( 'NONE', #4720, #2877, #931, .T. ) ;
#7580 = CARTESIAN_POINT ( 'NONE',  ( -16.11976138926855739, 99.99999999999997158, 16.60078749809536447 ) ) ;
#7581 = CARTESIAN_POINT ( 'NONE',  ( 6.477538756577482459, 100.0000000000000000, 20.49684993083915430 ) ) ;
#7582 = CARTESIAN_POINT ( 'NONE',  ( 4.739008722453744049, 99.50000000000001421, -24.06821587619827696 ) ) ;
#7583 = DIRECTION ( 'NONE',  ( -0.000000000000000000, -1.000000000000000000, -0.000000000000000000 ) ) ;
#7584 = CARTESIAN_POINT ( 'NONE',  ( -21.11719860449141351, 99.50000000000002842, -9.425423427278841970 ) ) ;
#7585 = CARTESIAN_POINT ( 'NONE',  ( 4.835062408351179286, 100.0000000000000000, -21.79588013901878440 ) ) ;
#7586 = ORIENTED_EDGE ( 'NONE', *, *, #1352, .F. ) ;
#7587 = CARTESIAN_POINT ( 'NONE',  ( 0.000000000000000000, 100.0000000000000000, 18.00000000000000000 ) ) ;
#7588 = CARTESIAN_POINT ( 'NONE',  ( -15.62751930918662069, 99.49999999999998579, 15.20915780906945436 ) ) ;
#7589 = CARTESIAN_POINT ( 'NONE',  ( -16.38049141020750099, 99.50000000000004263, 14.97568473612765416 ) ) ;
#7590 = CARTESIAN_POINT ( 'NONE',  ( 9.342627931057743140, 99.99999999999994316, 21.59831790269294771 ) ) ;
#7591 = CARTESIAN_POINT ( 'NONE',  ( 3.058419780146050648, 99.50000000000000000, -23.12871267107006545 ) ) ;
#7592 = ORIENTED_EDGE ( 'NONE', *, *, #7355, .F. ) ;
#7593 = EDGE_CURVE ( 'NONE', #4302, #6802, #3376, .T. ) ;
#7594 = CARTESIAN_POINT ( 'NONE',  ( 4.901590909071964042, 100.0000000000000000, -23.62641080846013608 ) ) ;
#7595 = CARTESIAN_POINT ( 'NONE',  ( -2.256430356250000102, -1.640624999385482896, -1.302750673588580321 ) ) ;
#7596 = ORIENTED_EDGE ( 'NONE', *, *, #1580, .T. ) ;
#7597 = CARTESIAN_POINT ( 'NONE',  ( 4.457146071884139360, 99.50000000000001421, -24.28472590373185724 ) ) ;
#7598 = LINE ( 'NONE', #8559, #6123 ) ;
#7599 = AXIS2_PLACEMENT_3D ( 'NONE', #4965, #5116, #9154 ) ;
#7600 = CARTESIAN_POINT ( 'NONE',  ( 3.434779879277784609, 99.50000000000001421, -23.17575050830969374 ) ) ;
#7601 = CARTESIAN_POINT ( 'NONE',  ( 0.000000000000000000, 72.50000000000001421, 0.000000000000000000 ) ) ;
#7602 = EDGE_CURVE ( 'NONE', #2877, #4679, #5886, .T. ) ;
#7603 = EDGE_CURVE ( 'NONE', #7033, #8764, #1801, .T. ) ;
#7604 = EDGE_CURVE ( 'NONE', #7920, #1900, #2598, .T. ) ;
#7605 = ORIENTED_EDGE ( 'NONE', *, *, #9018, .F. ) ;
#7606 = CARTESIAN_POINT ( 'NONE',  ( -4.959819536546781389E-15, 1.999999997815050445, 27.00000000000000355 ) ) ;
#7607 = CARTESIAN_POINT ( 'NONE',  ( -27.00000000000000355, 1.149999999999999689, -11.18376618407357270 ) ) ;
#7608 = CIRCLE ( 'NONE', #7286, 23.99999999999999645 ) ;
#7609 = ORIENTED_EDGE ( 'NONE', *, *, #4381, .T. ) ;
#7610 = CARTESIAN_POINT ( 'NONE',  ( 4.486604876299897349, 99.50000000000000000, -21.85617661337775885 ) ) ;
#7611 = CARTESIAN_POINT ( 'NONE',  ( -27.43301270000000969, 3.999999998907525001, 11.36312591709335429 ) ) ;
#7612 = CARTESIAN_POINT ( 'NONE',  ( -18.01369080470046313, 99.50000000000000000, 17.15556831233607937 ) ) ;
#7613 = DIRECTION ( 'NONE',  ( -0.000000000000000000, 1.000000000000000000, -0.000000000000000000 ) ) ;
#7614 = VECTOR ( 'NONE', #1283, 1000.000000000000227 ) ;
#7615 = CARTESIAN_POINT ( 'NONE',  ( 9.164845778125666698, 99.50000000000001421, 19.62003801130714820 ) ) ;
#7616 = CARTESIAN_POINT ( 'NONE',  ( 0.000000000000000000, -20.00000000000000000, 0.000000000000000000 ) ) ;
#7617 = FACE_OUTER_BOUND ( 'NONE', #8557, .T. ) ;
#7618 = SURFACE_SIDE_STYLE ('',( #3437 ) ) ;
#7619 = VERTEX_POINT ( 'NONE', #5786 ) ;
#7620 = FACE_OUTER_BOUND ( 'NONE', #4683, .T. ) ;
#7621 = CARTESIAN_POINT ( 'NONE',  ( 19.39806930854668110, 0.4499999989075251783, -19.39806930854668110 ) ) ;
#7622 = ORIENTED_EDGE ( 'NONE', *, *, #2573, .T. ) ;
#7623 = AXIS2_PLACEMENT_3D ( 'NONE', #2599, #2746, #1952 ) ;
#7624 = AXIS2_PLACEMENT_3D ( 'NONE', #1894, #4993, #1750 ) ;
#7625 = CARTESIAN_POINT ( 'NONE',  ( -1.767625397874844694E-16, -1.012499999999999956, -2.886751345948128655 ) ) ;
#7626 = APPLICATION_PROTOCOL_DEFINITION ( 'draft international standard', 'automotive_design', 1998, #10152 ) ;
#7627 = CARTESIAN_POINT ( 'NONE',  ( -9.703070624755296135E-15, -3.937500000000000888, 2.500000000000000444 ) ) ;
#7628 = CARTESIAN_POINT ( 'NONE',  ( 1.128215178125001161, -2.803124999385482319, 1.954126010382870815 ) ) ;
#7629 = CARTESIAN_POINT ( 'NONE',  ( 4.906732565843439531, 99.50000000000001421, -23.57187248890526376 ) ) ;
#7630 = CARTESIAN_POINT ( 'NONE',  ( 11.36312591709336139, 3.699999998907525622, -27.43301270000000258 ) ) ;
#7631 = ORIENTED_EDGE ( 'NONE', *, *, #6677, .F. ) ;
#7632 = CARTESIAN_POINT ( 'NONE',  ( 8.644881627383616873, 99.99999999999995737, 19.60534525227960145 ) ) ;
#7633 = MECHANICAL_DESIGN_GEOMETRIC_PRESENTATION_REPRESENTATION (  '', ( #1947 ), #10335 ) ;
#7634 = CARTESIAN_POINT ( 'NONE',  ( 4.054941747578200584, 99.49999999999998579, -24.36678493958047298 ) ) ;
#7635 = CARTESIAN_POINT ( 'NONE',  ( 7.729958523985794194, 100.0000000000000142, 20.63140804260154937 ) ) ;
#7636 = CARTESIAN_POINT ( 'NONE',  ( 0.000000000000000000, 87.00000000000001421, -7.500000000000000000 ) ) ;
#7637 = CARTESIAN_POINT ( 'NONE',  ( 4.786228327491940187E-16, -2.278124999385482852, 2.605501347177161087 ) ) ;
#7638 = DIRECTION ( 'NONE',  ( 0.000000000000000000, 0.000000000000000000, -1.000000000000000000 ) ) ;
#7639 = VERTEX_POINT ( 'NONE', #2645 ) ;
#7640 = ADVANCED_FACE ( 'NONE', ( #8194, #4216 ), #7445, .T. ) ;
#7641 = LINE ( 'NONE', #537, #6964 ) ;
#7642 = CARTESIAN_POINT ( 'NONE',  ( -19.39806930854668465, 2.349999998907525534, 19.39806930854667755 ) ) ;
#7643 = EDGE_CURVE ( 'NONE', #7824, #7095, #8099, .T. ) ;
#7644 =( NAMED_UNIT ( * ) PLANE_ANGLE_UNIT ( ) SI_UNIT ( $, .RADIAN. ) );
#7645 = ORIENTED_EDGE ( 'NONE', *, *, #2850, .T. ) ;
#7646 = LINE ( 'NONE', #4566, #3582 ) ;
#7647 = CARTESIAN_POINT ( 'NONE',  ( 9.576498344683301411, 99.99999999999992895, 20.78592410672095880 ) ) ;
#7648 = AXIS2_PLACEMENT_3D ( 'NONE', #844, #4035, #4870 ) ;
#7649 = DIRECTION ( 'NONE',  ( 1.000000000000000000, 0.000000000000000000, 0.000000000000000000 ) ) ;
#7650 = ORIENTED_EDGE ( 'NONE', *, *, #956, .T. ) ;
#7651 = CARTESIAN_POINT ( 'NONE',  ( -16.24524625128438515, 99.50000000000002842, 16.53274063862002308 ) ) ;
#7652 = CARTESIAN_POINT ( 'NONE',  ( -1.595409442497313560E-16, -2.165624999385483029, -2.605501347177161087 ) ) ;
#7653 = EDGE_LOOP ( 'NONE', ( #5863, #4940 ) ) ;
#7654 = VECTOR ( 'NONE', #3239, 1000.000000000000114 ) ;
#7655 = CARTESIAN_POINT ( 'NONE',  ( 4.232798786556307036, 99.50000000000000000, -24.34936571594186105 ) ) ;
#7656 = CARTESIAN_POINT ( 'NONE',  ( 2.500000000000000000, -0.6375000000000000666, -1.443375672974065438 ) ) ;
#7657 = LINE ( 'NONE', #550, #727 ) ;
#7658 = EDGE_CURVE ( 'NONE', #1454, #8208, #9029, .T. ) ;
#7659 = CARTESIAN_POINT ( 'NONE',  ( 3.061616997868382648E-16, -5.000000000000000000, 2.499999999999999556 ) ) ;
#7660 = CARTESIAN_POINT ( 'NONE',  ( 2.958578797724396026, 100.0000000000000000, -23.36432507653281121 ) ) ;
#7661 = EDGE_LOOP ( 'NONE', ( #1735, #1174, #7622, #4282 ) ) ;
#7662 = B_SPLINE_CURVE_WITH_KNOTS ( 'NONE', 3,
 ( #8805, #803, #7327, #63 ),
 .UNSPECIFIED., .F., .F.,
 ( 4, 4 ),
 ( 0.000000000000000000, 1.000000000000000000 ),
 .UNSPECIFIED. ) ;
#7663 = CARTESIAN_POINT ( 'NONE',  ( 4.295198626299898237, 99.50000000000001421, -24.68029520312135361 ) ) ;
#7664 = CARTESIAN_POINT ( 'NONE',  ( -19.75840245672548789, 100.0000000000000000, -8.735905494466331689 ) ) ;
#7665 = CARTESIAN_POINT ( 'NONE',  ( 0.000000000000000000, 100.0000000000000000, 0.000000000000000000 ) ) ;
#7666 = VERTEX_POINT ( 'NONE', #286 ) ;
#7667 = LINE ( 'NONE', #9918, #3241 ) ;
#7668 = CARTESIAN_POINT ( 'NONE',  ( -27.43301270000000258, 3.099999998907525089, -11.36312591709336317 ) ) ;
#7669 = CARTESIAN_POINT ( 'NONE',  ( -2.256430356250000102, -0.5906249993854829627, 0.000000000000000000 ) ) ;
#7670 = CARTESIAN_POINT ( 'NONE',  ( 9.820792995160310568, 99.50000000000001421, 20.21220011423141116 ) ) ;
#7671 = PRODUCT_DEFINITION_SHAPE ( 'NONE', 'NONE',  #10370 ) ;
#7672 = VERTEX_POINT ( 'NONE', #3478 ) ;
#7673 = DIRECTION ( 'NONE',  ( 0.000000000000000000, -1.000000000000000000, 0.000000000000000000 ) ) ;
#7674 = CARTESIAN_POINT ( 'NONE',  ( 5.243816414761435674, 99.50000000000000000, -23.48558366465980995 ) ) ;
#7675 = SURFACE_STYLE_FILL_AREA ( #10029 ) ;
#7676 = CARTESIAN_POINT ( 'NONE',  ( 0.000000000000000000, 5.000000000000000000, 0.000000000000000000 ) ) ;
#7677 = B_SPLINE_CURVE_WITH_KNOTS ( 'NONE', 3,
 ( #8644, #4661, #4549, #10159, #6172, #5507, #7851, #1305, #681, #3717, #6284, #4495, #9481, #9309, #2141, #5399, #8696, #2307, #1357 ),
 .UNSPECIFIED., .F., .F.,
 ( 4, 1, 1, 1, 1, 1, 1, 1, 1, 1, 1, 1, 1, 1, 1, 1, 4 ),
 ( 0.000000000000000000, 0.06363772181477481138, 0.1253661190162797812, 0.1854850957718461035, 0.2454326483351531030, 0.3054881917026986415, 0.3659564384638642753, 0.4275766838088623234, 0.4913505196498278993, 0.5556437034595619329, 0.6183735394983103095, 0.6802114403575724166, 0.7422401234104337719, 0.8041288543812358247, 0.8678488776753463529, 0.9326351893241184854, 1.000000000000000000 ),
 .UNSPECIFIED. ) ;
#7678 = ORIENTED_EDGE ( 'NONE', *, *, #2551, .F. ) ;
#7679 = CARTESIAN_POINT ( 'NONE',  ( 9.248677610544923766, 100.0000000000000000, 22.83089001807756446 ) ) ;
#7680 = CARTESIAN_POINT ( 'NONE',  ( -5.039362679103552881E-15, 0.9499999989075252893, 27.43301270000000258 ) ) ;
#7681 = EDGE_CURVE ( 'NONE', #5894, #728, #6664, .T. ) ;
#7682 = CARTESIAN_POINT ( 'NONE',  ( -2.499999999999999556, -2.212499999999999467, 1.443375672974065882 ) ) ;
#7683 = SHAPE_DEFINITION_REPRESENTATION ( #7191, #5481 ) ;
#7684 = CARTESIAN_POINT ( 'NONE',  ( -22.33111803333905243, 99.49999999999997158, -9.558150950182401573 ) ) ;
#7685 = CARTESIAN_POINT ( 'NONE',  ( 0.000000000000000000, 100.0000000000000000, 0.000000000000000000 ) ) ;
#7686 = CARTESIAN_POINT ( 'NONE',  ( -2.256430356249999214, -1.565624999385482718, 1.302750673588581876 ) ) ;
#7687 = CARTESIAN_POINT ( 'NONE',  ( 11.36312591709336139, 4.399999998907525800, -27.43301270000000258 ) ) ;
#7688 = CARTESIAN_POINT ( 'NONE',  ( 19.39806930854667399, 1.049999998907525045, 19.39806930854668465 ) ) ;
#7689 = ORIENTED_EDGE ( 'NONE', *, *, #7457, .T. ) ;
#7690 = UNCERTAINTY_MEASURE_WITH_UNIT (LENGTH_MEASURE( 1.000000000000000082E-05 ), #1042, 'distance_accuracy_value', 'NONE');
#7691 = CARTESIAN_POINT ( 'NONE',  ( 1.249999999999999334, -1.949999999999999956, -2.165063509461096825 ) ) ;
#7692 = CARTESIAN_POINT ( 'NONE',  ( 2.939152317953648289E-15, 97.00000000000000000, 24.00000000000000355 ) ) ;
#7693 = CARTESIAN_POINT ( 'NONE',  ( 3.203979444200292015, 99.50000000000000000, -21.29640115293693725 ) ) ;
#7694 = CARTESIAN_POINT ( 'NONE',  ( 3.296462644833695776, 100.0000000000000142, -23.81854410834942115 ) ) ;
#7695 = AXIS2_PLACEMENT_3D ( 'NONE', #7511, #2608, #7360 ) ;
#7696 = ORIENTED_EDGE ( 'NONE', *, *, #6983, .F. ) ;
#7697 = CARTESIAN_POINT ( 'NONE',  ( -1.128215178124998497, -1.415624999385482807, 1.954126010382872147 ) ) ;
#7698 = CARTESIAN_POINT ( 'NONE',  ( 4.793167276645844410, 99.49999999999998579, -21.69837440717521204 ) ) ;
#7699 = EDGE_LOOP ( 'NONE', ( #6110, #4621, #1501, #8543 ) ) ;
#7700 = CARTESIAN_POINT ( 'NONE',  ( 2.256430356249999658, -0.3281249993854829516, -1.302750673588581432 ) ) ;
#7701 = CARTESIAN_POINT ( 'NONE',  ( 19.39806930854668110, 1.149999998907525356, -19.39806930854668110 ) ) ;
#7702 = SHAPE_REPRESENTATION_RELATIONSHIP ( 'NONE' , 'NONE' ,  #1584, #7366 ) ;
#7703 = EDGE_LOOP ( 'NONE', ( #4770, #7631, #5488, #3191 ) ) ;
#7704 = CARTESIAN_POINT ( 'NONE',  ( 1.670949432750432147E-15, 5.166666665938350000, -27.28867513333333505 ) ) ;
#7705 = CARTESIAN_POINT ( 'NONE',  ( -27.00000000000001421, 0.4500000000000000666, 11.18376618407356382 ) ) ;
#7706 = CARTESIAN_POINT ( 'NONE',  ( 9.482997300390421103, 100.0000000000000284, 20.28643943712827991 ) ) ;
#7707 = ORIENTED_EDGE ( 'NONE', *, *, #5107, .T. ) ;
#7708 = ORIENTED_EDGE ( 'NONE', *, *, #2294, .T. ) ;
#7709 = CARTESIAN_POINT ( 'NONE',  ( 4.829054701479813083, 100.0000000000000000, -23.91032069601275367 ) ) ;
#7710 = CARTESIAN_POINT ( 'NONE',  ( -2.256430356250000102, -0.7406249993854829849, -1.302750673588580321 ) ) ;
#7711 = VERTEX_POINT ( 'NONE', #9081 ) ;
#7712 = DIRECTION ( 'NONE',  ( -0.000000000000000000, -1.000000000000000000, -0.000000000000000000 ) ) ;
#7713 = CARTESIAN_POINT ( 'NONE',  ( -21.66466628782423243, 99.50000000000001421, -9.640935998098070669 ) ) ;
#7714 = CARTESIAN_POINT ( 'NONE',  ( -2.256430356250000102, -0.7031249993854828961, 0.000000000000000000 ) ) ;
#7715 = CARTESIAN_POINT ( 'NONE',  ( 5.047889085735837611, 99.50000000000001421, -24.22022158424849536 ) ) ;
#7716 = VECTOR ( 'NONE', #1820, 1000.000000000000000 ) ;
#7717 = EDGE_CURVE ( 'NONE', #8640, #224, #1896, .T. ) ;
#7718 = CARTESIAN_POINT ( 'NONE',  ( -2.500000000000000000, -0.4312499987709658700, -1.443375672974064106 ) ) ;
#7719 = CARTESIAN_POINT ( 'NONE',  ( 0.000000000000000000, 70.00000000000000000, 0.000000000000000000 ) ) ;
#7720 = CARTESIAN_POINT ( 'NONE',  ( 11.18376618407357093, 0.9499999999999999556, -27.00000000000000355 ) ) ;
#7721 =( BOUNDED_CURVE ( )  B_SPLINE_CURVE ( 2, ( #2700, #6041, #9231, #2805, #2063, #5257, #7556, #4475, #6721 ),
 .UNSPECIFIED., .F., .F. ) 
 B_SPLINE_CURVE_WITH_KNOTS ( ( 3, 2, 2, 2, 3 ),
 ( 0.1071428571428571369, 0.1250000000000000000, 0.1428571428571428492, 0.1607142857142857262, 0.1785714285714285754 ),
 .UNSPECIFIED. ) 
 CURVE ( )  GEOMETRIC_REPRESENTATION_ITEM ( )  RATIONAL_B_SPLINE_CURVE ( ( 1.000000000000000000, 0.9238795325112867385, 1.000000000000000000, 0.9238795325112867385, 1.000000000000000000, 0.9238795325112867385, 1.000000000000000000, 0.9238795325112867385, 1.000000000000000000 ) ) 
 REPRESENTATION_ITEM ( '' )  );
#7722 = ORIENTED_EDGE ( 'NONE', *, *, #2695, .T. ) ;
#7723 = PLANE ( 'NONE',  #730 ) ;
#7724 = CARTESIAN_POINT ( 'NONE',  ( -1.249999999999998224, -4.368749998770964815, 2.165063509461097713 ) ) ;
#7725 = CARTESIAN_POINT ( 'NONE',  ( -2.256430356249999214, -2.353124999385482585, 1.302750673588581876 ) ) ;
#7726 = AXIS2_PLACEMENT_3D ( 'NONE', #8298, #9920, #6826 ) ;
#7727 = CARTESIAN_POINT ( 'NONE',  ( 9.834295043520187463, 99.50000000000002842, 21.14079655679390513 ) ) ;
#7728 = VERTEX_POINT ( 'NONE', #499 ) ;
#7729 = DIRECTION ( 'NONE',  ( 0.3368601548094422582, 0.000000000000000000, -0.9415546909775122097 ) ) ;
#7730 = CARTESIAN_POINT ( 'NONE',  ( 5.098880966732203035, 99.50000000000000000, -24.13374913903897223 ) ) ;
#7731 = CARTESIAN_POINT ( 'NONE',  ( -22.57971655928959365, 100.0000000000000000, -10.84768434062017839 ) ) ;
#7732 = FACE_OUTER_BOUND ( 'NONE', #2923, .T. ) ;
#7733 = VECTOR ( 'NONE', #960, 1000.000000000000000 ) ;
#7734 = ORIENTED_EDGE ( 'NONE', *, *, #2031, .F. ) ;
#7735 = CARTESIAN_POINT ( 'NONE',  ( -15.43596444985078975, 99.50000000000002842, 15.30036492734783593 ) ) ;
#7736 = CARTESIAN_POINT ( 'NONE',  ( -27.43301270000000258, 0.6999999989075252893, -11.36312591709336317 ) ) ;
#7737 = ORIENTED_EDGE ( 'NONE', *, *, #8492, .F. ) ;
#7738 = CARTESIAN_POINT ( 'NONE',  ( -2.500000000000000000, -2.699999999999999734, 0.000000000000000000 ) ) ;
#7739 = PRODUCT_CONTEXT ( 'NONE', #4070, 'mechanical' ) ;
#7740 = LINE ( 'NONE', #573, #1861 ) ;
#7741 = CARTESIAN_POINT ( 'NONE',  ( 2.864934851235464208, 99.50000000000000000, -21.80148171563692827 ) ) ;
#7742 = CARTESIAN_POINT ( 'NONE',  ( -2.256430356249999214, -2.465624999385482852, 1.302750673588581876 ) ) ;
#7743 = EDGE_CURVE ( 'NONE', #5515, #4002, #6877, .T. ) ;
#7744 = CARTESIAN_POINT ( 'NONE',  ( -7.500000000000000000, 104.5000000000000142, 1.000000000000000222 ) ) ;
#7745 = CARTESIAN_POINT ( 'NONE',  ( 11.36312591709336139, 2.899999998907526244, -27.43301270000000258 ) ) ;
#7746 = AXIS2_PLACEMENT_3D ( 'NONE', #9264, #4561, #3782 ) ;
#7748 = ORIENTED_EDGE ( 'NONE', *, *, #5916, .F. ) ;
#7747 = VERTEX_POINT ( 'NONE', #5252 ) ;
#7749 = ADVANCED_FACE ( 'NONE', ( #3694 ), #3584, .T. ) ;
#7750 = CARTESIAN_POINT ( 'NONE',  ( -16.05266356869597644, 100.0000000000000000, 16.62382211633880047 ) ) ;
#7751 = LINE ( 'NONE', #3000, #2809 ) ;
#7752 = CARTESIAN_POINT ( 'NONE',  ( -16.63177974700816009, 99.50000000000000000, 16.59747536361813403 ) ) ;
#7753 = CARTESIAN_POINT ( 'NONE',  ( 3.735769352376668184, 99.99999999999998579, -24.30643046864489420 ) ) ;
#7754 = ORIENTED_EDGE ( 'NONE', *, *, #10299, .F. ) ;
#7755 = CARTESIAN_POINT ( 'NONE',  ( 1.128215178124999607, -1.190624999385482941, -1.954126010382871259 ) ) ;
#7756 = CARTESIAN_POINT ( 'NONE',  ( -2.256430356250000102, -0.1406249993854829794, 0.000000000000000000 ) ) ;
#7757 = EDGE_LOOP ( 'NONE', ( #7898, #1399, #8449, #2714 ) ) ;
#7758 = CARTESIAN_POINT ( 'NONE',  ( -0.6698729810778069060, -1.386153809338631415, -2.500000000000000000 ) ) ;
#7759 = CARTESIAN_POINT ( 'NONE',  ( 27.43301270000000258, 1.899999998907525134, -11.36312591709336139 ) ) ;
#7760 = VERTEX_POINT ( 'NONE', #5316 ) ;
#7761 = DIRECTION ( 'NONE',  ( 0.000000000000000000, -1.000000000000000000, 0.000000000000000000 ) ) ;
#7762 = CARTESIAN_POINT ( 'NONE',  ( -4.959819536546781389E-15, 2.200000000000000178, 27.00000000000000355 ) ) ;
#7763 = CARTESIAN_POINT ( 'NONE',  ( 9.182805720491336032, 99.50000000000000000, 20.00174565872165289 ) ) ;
#7764 = ORIENTED_EDGE ( 'NONE', *, *, #9344, .T. ) ;
#7765 = VERTEX_POINT ( 'NONE', #4420 ) ;
#7766 = CARTESIAN_POINT ( 'NONE',  ( -16.49419651247312046, 99.49999999999998579, 15.57134447358898477 ) ) ;
#7767 = CARTESIAN_POINT ( 'NONE',  ( -15.31787750341841559, 99.50000000000000000, 16.43551622900274722 ) ) ;
#7768 = CARTESIAN_POINT ( 'NONE',  ( 2.256430356249999658, -4.490624999385483207, -1.302750673588581432 ) ) ;
#7769 = VERTEX_POINT ( 'NONE', #7606 ) ;
#7770 = CARTESIAN_POINT ( 'NONE',  ( 0.000000000000000000, 87.00000000000001421, 0.000000000000000000 ) ) ;
#7771 = PLANE ( 'NONE',  #2202 ) ;
#7772 = PRODUCT ( 'gas generator', 'gas generator', '', ( #1248 ) ) ;
#7773 = CARTESIAN_POINT ( 'NONE',  ( -1.128215178124998497, -1.078124999385482674, 1.954126010382872147 ) ) ;
#7774 = CARTESIAN_POINT ( 'NONE',  ( 3.411785164761435674, 100.0000000000000000, -22.76693382491622231 ) ) ;
#7775 = CARTESIAN_POINT ( 'NONE',  ( 1.249999999999999334, -0.5437499987709658589, -2.165063509461096825 ) ) ;
#7776 = CIRCLE ( 'NONE', #8624, 2.500000000000000000 ) ;
#7777 = CARTESIAN_POINT ( 'NONE',  ( -16.85368146453285831, 99.99999999999998579, 16.27421966797335529 ) ) ;
#7778 = DIRECTION ( 'NONE',  ( 0.000000000000000000, -1.000000000000000000, 0.000000000000000000 ) ) ;
#7779 = DIRECTION ( 'NONE',  ( 1.000000000000000000, 0.000000000000000000, 0.000000000000000000 ) ) ;
#7780 = CARTESIAN_POINT ( 'NONE',  ( -1.128215178125000273, -1.565624999385482941, -1.954126010382871259 ) ) ;
#7781 = EDGE_CURVE ( 'NONE', #9021, #669, #5089, .T. ) ;
#7782 = AXIS2_PLACEMENT_3D ( 'NONE', #8518, #7673, #564 ) ;
#7783 = CARTESIAN_POINT ( 'NONE',  ( -21.20585021321354802, 100.0000000000000568, -9.381045134209834657 ) ) ;
#7784 = CARTESIAN_POINT ( 'NONE',  ( 9.263267005978743640, 99.49999999999998579, 19.65676951151765905 ) ) ;
#7785 = PRESENTATION_STYLE_ASSIGNMENT (( #3704 ) ) ;
#7786 = AXIS2_PLACEMENT_3D ( 'NONE', #3117, #4511, #594 ) ;
#7787 =( BOUNDED_CURVE ( )  B_SPLINE_CURVE ( 2, ( #8958, #4832, #5622, #5021, #1734, #8218, #4927, #5675, #216 ),
 .UNSPECIFIED., .F., .F. ) 
 B_SPLINE_CURVE_WITH_KNOTS ( ( 3, 2, 2, 2, 3 ),
 ( 0.2500000000000000000, 0.2678571428571428492, 0.2857142857142856984, 0.3035714285714285476, 0.3214285714285714524 ),
 .UNSPECIFIED. ) 
 CURVE ( )  GEOMETRIC_REPRESENTATION_ITEM ( )  RATIONAL_B_SPLINE_CURVE ( ( 1.000000000000000000, 0.9238795325112867385, 1.000000000000000000, 0.9238795325112867385, 1.000000000000000000, 0.9238795325112867385, 1.000000000000000000, 0.9238795325112867385, 1.000000000000000000 ) ) 
 REPRESENTATION_ITEM ( '' )  );
#7788 = DIRECTION ( 'NONE',  ( -0.000000000000000000, -1.000000000000000000, -0.000000000000000000 ) ) ;
#7789 = VERTEX_POINT ( 'NONE', #9967 ) ;
#7790 = CARTESIAN_POINT ( 'NONE',  ( -15.32348647777738826, 100.0000000000000000, 15.39505148541300450 ) ) ;
#7791 = CARTESIAN_POINT ( 'NONE',  ( 9.248677610544923766, 99.50000000000000000, 22.83089001807756446 ) ) ;
#7792 = ORIENTED_EDGE ( 'NONE', *, *, #7658, .F. ) ;
#7793 = CARTESIAN_POINT ( 'NONE',  ( -1.249999999999998224, -4.424999999999998934, 2.165063509461097713 ) ) ;
#7794 = EDGE_CURVE ( 'NONE', #3612, #1490, #6150, .T. ) ;
#7795 = CARTESIAN_POINT ( 'NONE',  ( 3.681717055787076642, 99.99999999999997158, -21.09125273517263111 ) ) ;
#7796 = CARTESIAN_POINT ( 'NONE',  ( -1.128215178125000273, -2.128124999385482496, -1.954126010382871259 ) ) ;
#7797 = CARTESIAN_POINT ( 'NONE',  ( 1.653273178848927064E-15, 0.7999999978150503788, -27.00000000000000355 ) ) ;
#7798 = CARTESIAN_POINT ( 'NONE',  ( 27.43301270000000258, 1.149999998907525356, 0.000000000000000000 ) ) ;
#7799 = UNCERTAINTY_MEASURE_WITH_UNIT (LENGTH_MEASURE( 1.000000000000000082E-05 ), #6798, 'distance_accuracy_value', 'NONE');
#7800 = CARTESIAN_POINT ( 'NONE',  ( -16.30427144417478402, 99.99999999999998579, 16.48895498912494517 ) ) ;
#7801 = DIRECTION ( 'NONE',  ( 0.000000000000000000, -1.000000000000000000, 0.000000000000000000 ) ) ;
#7802 = CARTESIAN_POINT ( 'NONE',  ( 3.231466532446834350, 99.49999999999997158, -21.81145066552309686 ) ) ;
#7803 = CARTESIAN_POINT ( 'NONE',  ( -16.12578516900833137, 100.0000000000000142, 15.23469143358620492 ) ) ;
#7804 = VECTOR ( 'NONE', #2972, 1000.000000000000000 ) ;
#7805 = PRODUCT_DEFINITION ( 'UNKNOWN', '', #6984, #2996 ) ;
#7806 = CARTESIAN_POINT ( 'NONE',  ( 2.256430356250000102, -1.715624999385482852, -2.763330213280484622E-16 ) ) ;
#7807 = CARTESIAN_POINT ( 'NONE',  ( 4.504418077186241653, 99.50000000000004263, -21.31258943653750393 ) ) ;
#7808 = ORIENTED_EDGE ( 'NONE', *, *, #5959, .F. ) ;
#7809 = VERTEX_POINT ( 'NONE', #6989 ) ;
#7810 = CARTESIAN_POINT ( 'NONE',  ( 2.256430356249999658, -1.228124999385483029, -1.302750673588581432 ) ) ;
#7811 = CARTESIAN_POINT ( 'NONE',  ( -11.36312591709337383, 3.199999998907524734, 27.43301269999999548 ) ) ;
#7812 = ORIENTED_EDGE ( 'NONE', *, *, #2158, .T. ) ;
#7813 = EDGE_CURVE ( 'NONE', #3209, #7282, #1227, .T. ) ;
#7814 = AXIS2_PLACEMENT_3D ( 'NONE', #5349, #476, #8538 ) ;
#7815 = CARTESIAN_POINT ( 'NONE',  ( -4.357666448243394824E-15, -2.981249998770965526, 2.500000000000000000 ) ) ;
#7816 = CARTESIAN_POINT ( 'NONE',  ( 27.00000000000000355, 0.000000000000000000, 0.000000000000000000 ) ) ;
#7817 = CARTESIAN_POINT ( 'NONE',  ( 9.482997300390421103, 99.50000000000000000, 20.28643943712827991 ) ) ;
#7818 = VERTEX_POINT ( 'NONE', #2799 ) ;
#7819 = VERTEX_POINT ( 'NONE', #4582 ) ;
#7820 = CARTESIAN_POINT ( 'NONE',  ( -15.15871127190382417, 99.50000000000000000, 15.63231653451427761 ) ) ;
#7821 = CARTESIAN_POINT ( 'NONE',  ( 8.467217662126737210, 99.50000000000001421, 20.02246181083229004 ) ) ;
#7822 = CARTESIAN_POINT ( 'NONE',  ( 2.256430356250000102, -4.528124999385481964, -2.763330213280484622E-16 ) ) ;
#7823 = ORIENTED_EDGE ( 'NONE', *, *, #7794, .T. ) ;
#7824 = VERTEX_POINT ( 'NONE', #4470 ) ;
#7825 = FACE_BOUND ( 'NONE', #5526, .T. ) ;
#7826 = CARTESIAN_POINT ( 'NONE',  ( 1.250000000000001110, -0.2999999999999999889, 2.165063509461096380 ) ) ;
#7827 = ADVANCED_FACE ( 'NONE', ( #6769 ), #2707, .T. ) ;
#7828 = CARTESIAN_POINT ( 'NONE',  ( 4.786228327491940187E-16, -1.490624999385482541, 2.605501347177161087 ) ) ;
#7829 = CARTESIAN_POINT ( 'NONE',  ( 2.940192896829773250, 100.0000000000000142, -23.44521981770616037 ) ) ;
#7830 = FACE_OUTER_BOUND ( 'NONE', #1177, .T. ) ;
#7831 = VECTOR ( 'NONE', #9257, 1000.000000000000000 ) ;
#7832 = CARTESIAN_POINT ( 'NONE',  ( -1.767625397874844694E-16, -1.406249998770965570, -2.886751345948128655 ) ) ;
#7833 = CARTESIAN_POINT ( 'NONE',  ( 4.386516977709190357, 99.50000000000004263, -24.31220192127581825 ) ) ;
#7834 = DIRECTION ( 'NONE',  ( 0.000000000000000000, -0.000000000000000000, -1.000000000000000000 ) ) ;
#7835 = ORIENTED_EDGE ( 'NONE', *, *, #6832, .T. ) ;
#7836 = CARTESIAN_POINT ( 'NONE',  ( 3.061616997868383141E-16, 0.000000000000000000, 2.500000000000000000 ) ) ;
#7837 = CARTESIAN_POINT ( 'NONE',  ( 2.256430356250000102, -1.265624999385482896, -2.763330213280484622E-16 ) ) ;
#7838 = ORIENTED_EDGE ( 'NONE', *, *, #385, .F. ) ;
#7839 = CARTESIAN_POINT ( 'NONE',  ( -20.82968571475833031, 100.0000000000000142, -9.677916414284339908 ) ) ;
#7840 = CARTESIAN_POINT ( 'NONE',  ( 8.644881627383616873, 99.49999999999995737, 19.60534525227960145 ) ) ;
#7841 = ADVANCED_FACE ( 'NONE', ( #8763 ), #7975, .T. ) ;
#7842 =( NAMED_UNIT ( * ) SI_UNIT ( $, .STERADIAN. ) SOLID_ANGLE_UNIT ( ) );
#7843 = DIRECTION ( 'NONE',  ( -0.9985315370676781654, 0.000000000000000000, 0.05417351272771728926 ) ) ;
#7844 = ORIENTED_EDGE ( 'NONE', *, *, #3252, .T. ) ;
#7845 = LINE ( 'NONE', #568, #8471 ) ;
#7846 = CARTESIAN_POINT ( 'NONE',  ( -11.36312591709335962, 3.799999998907525711, -27.43301270000000258 ) ) ;
#7847 = VERTEX_POINT ( 'NONE', #8307 ) ;
#7848 = FILL_AREA_STYLE ('',( #4658 ) ) ;
#7849 = CARTESIAN_POINT ( 'NONE',  ( 6.477538756577482459, 99.50000000000000000, 20.49684993083915430 ) ) ;
#7850 = CARTESIAN_POINT ( 'NONE',  ( -1.128215178124998497, -1.078124999385482674, 1.954126010382872147 ) ) ;
#7851 = CARTESIAN_POINT ( 'NONE',  ( -16.88522588321459494, 99.50000000000002842, 16.18266969485829421 ) ) ;
#7852 = CARTESIAN_POINT ( 'NONE',  ( 19.39806930854667399, 3.449999998907525622, 19.39806930854668465 ) ) ;
#7853 =( BOUNDED_CURVE ( )  B_SPLINE_CURVE ( 2, ( #455, #3651, #6829, #6214, #9294, #3814, #6997, #5328, #1344 ),
 .UNSPECIFIED., .F., .T. ) 
 B_SPLINE_CURVE_WITH_KNOTS ( ( 3, 2, 2, 2, 3 ),
 ( 0.06250000000000000000, 0.06944444444444444753, 0.08333333333333332871, 0.09722222222222222376, 0.1041666666666666713 ),
 .UNSPECIFIED. ) 
 CURVE ( )  GEOMETRIC_REPRESENTATION_ITEM ( )  RATIONAL_B_SPLINE_CURVE ( ( 0.9330127018922194093, 0.9330127018922194093, 1.000000000000000000, 0.8660254037844387076, 1.000000000000000000, 0.8660254037844387076, 1.000000000000000000, 0.9330127018922192983, 0.9330127018922194093 ) ) 
 REPRESENTATION_ITEM ( '' )  );
#7854 = CARTESIAN_POINT ( 'NONE',  ( -15.10617644529808423, 100.0000000000000000, 15.98944417891004477 ) ) ;
#7855 = CARTESIAN_POINT ( 'NONE',  ( -2.500000000000000000, -3.093749998770965348, 0.000000000000000000 ) ) ;
#7856 = CARTESIAN_POINT ( 'NONE',  ( 3.638175769014108774, 99.49999999999998579, -21.10017783766535970 ) ) ;
#7857 = EDGE_CURVE ( 'NONE', #5955, #9728, #1799, .T. ) ;
#7858 = B_SPLINE_SURFACE_WITH_KNOTS ( 'NONE', 3, 1, ( 
 ( #8761, #597 ),
 ( #756, #1586 ),
 ( #7821, #4778 ),
 ( #3121, #7974 ),
 ( #6247, #10287 ),
 ( #8664, #650 ),
 ( #7030, #1533 ),
 ( #807, #5421 ),
 ( #4729, #10338 ),
 ( #3793, #4001 ),
 ( #8611, #2277 ),
 ( #7922, #4571 ),
 ( #10120, #1487 ),
 ( #4681, #1435 ),
 ( #6138, #7082 ),
 ( #6305, #3169 ),
 ( #5364, #2163 ),
 ( #3948, #6978 ),
 ( #8553, #9502 ) ),
 .UNSPECIFIED., .F., .F., .F.,
 ( 4, 1, 1, 1, 1, 1, 1, 1, 1, 1, 1, 1, 1, 1, 1, 1, 4 ),
 ( 2, 2 ),
 ( 0.000000000000000000, 0.06282509715607415002, 0.1231380613775250599, 0.1822388757841713336, 0.2396184841454026548, 0.2973605923678978580, 0.3541959668311244203, 0.4122907788200148582, 0.4717534157231769720, 0.5322282553174864095, 0.5926403291039165078, 0.6546871955647078911, 0.7179012776534754448, 0.7839155840457150415, 0.8527518695723632636, 0.9242989153657757972, 1.000000000000000000 ),
 ( 0.000000000000000000, 1.000000000000000000 ),
 .UNSPECIFIED. ) ;
#7859 = CARTESIAN_POINT ( 'NONE',  ( 27.00000000000000355, 4.049999999999999822, -11.18376618407356915 ) ) ;
#7860 = CARTESIAN_POINT ( 'NONE',  ( 1.128215178125001161, -2.240624999385482763, 1.954126010382870815 ) ) ;
#7861 = CARTESIAN_POINT ( 'NONE',  ( 3.712044765110731337, 99.99999999999998579, -21.08683700305641651 ) ) ;
#7862 = ORIENTED_EDGE ( 'NONE', *, *, #7977, .T. ) ;
#7863 = CARTESIAN_POINT ( 'NONE',  ( -2.256430356250000102, -1.978124999385482807, -1.302750673588580321 ) ) ;
#7864 = CARTESIAN_POINT ( 'NONE',  ( -5.039362679103552881E-15, 3.249999998907525001, 27.43301270000000258 ) ) ;
#7865 = CARTESIAN_POINT ( 'NONE',  ( -15.84712739808237103, 99.49999999999997158, 14.83079670662049310 ) ) ;
#7866 = CARTESIAN_POINT ( 'NONE',  ( 11.18376618407356915, 1.750000000000000222, -27.00000000000000355 ) ) ;
#7867 = CARTESIAN_POINT ( 'NONE',  ( 9.513000527211589841, 100.0000000000000284, 20.35102222961602436 ) ) ;
#7868 = ORIENTED_EDGE ( 'NONE', *, *, #4990, .T. ) ;
#7869 = CARTESIAN_POINT ( 'NONE',  ( -16.56313167360273297, 99.50000000000002842, 16.06491815633068398 ) ) ;
#7870 = CARTESIAN_POINT ( 'NONE',  ( -15.37123125604856710, 100.0000000000000142, 16.48683530611566539 ) ) ;
#7871 = CARTESIAN_POINT ( 'NONE',  ( 2.256430356249999658, -3.140624999385482674, -1.302750673588581432 ) ) ;
#7872 = VERTEX_POINT ( 'NONE', #1863 ) ;
#7873 = CARTESIAN_POINT ( 'NONE',  ( -5.039362679103552881E-15, 2.449999998907525178, 27.43301270000000258 ) ) ;
#7874 = DIRECTION ( 'NONE',  ( 0.000000000000000000, -1.000000000000000000, 0.000000000000000000 ) ) ;
#7875 = CARTESIAN_POINT ( 'NONE',  ( 1.128215178124999607, -2.653124999385482408, -1.954126010382871259 ) ) ;
#7876 = CARTESIAN_POINT ( 'NONE',  ( -27.00000000000001421, 3.650000000000000355, 11.18376618407356560 ) ) ;
#7877 = CARTESIAN_POINT ( 'NONE',  ( 11.18376618407357626, 4.449999997815051067, 27.00000000000000000 ) ) ;
#7878 = EDGE_CURVE ( 'NONE', #5471, #7399, #2642, .T. ) ;
#7879 = EDGE_CURVE ( 'NONE', #7425, #229, #3998, .T. ) ;
#7880 = ORIENTED_EDGE ( 'NONE', *, *, #7210, .T. ) ;
#7881 = CARTESIAN_POINT ( 'NONE',  ( 1.250000000000001110, -1.593749998770965792, 2.165063509461096380 ) ) ;
#7882 = ORIENTED_EDGE ( 'NONE', *, *, #8426, .T. ) ;
#7883 = CARTESIAN_POINT ( 'NONE',  ( 4.311343222282856047, 99.50000000000000000, -24.33387958695581688 ) ) ;
#7884 = CARTESIAN_POINT ( 'NONE',  ( 3.061616997868383043E-15, 87.00000000000001421, 25.00000000000000000 ) ) ;
#7885 = ORIENTED_EDGE ( 'NONE', *, *, #6211, .T. ) ;
#7886 = CARTESIAN_POINT ( 'NONE',  ( 0.6698729810778075722, -4.367403810567665801, 2.499999999999999556 ) ) ;
#7887 = CARTESIAN_POINT ( 'NONE',  ( 1.128215178125001161, -2.240624999385482763, 1.954126010382870815 ) ) ;
#7888 = ORIENTED_EDGE ( 'NONE', *, *, #7579, .T. ) ;
#7889 = AXIS2_PLACEMENT_3D ( 'NONE', #9515, #7779, #6209 ) ;
#7890 = VERTEX_POINT ( 'NONE', #1191 ) ;
#7891 = CARTESIAN_POINT ( 'NONE',  ( 2.924645347134957163, 99.50000000000001421, -23.60918035669702064 ) ) ;
#7892 = CARTESIAN_POINT ( 'NONE',  ( 9.725694684612619767, 99.50000000000000000, 20.03234812723199454 ) ) ;
#7893 =( LENGTH_UNIT ( ) NAMED_UNIT ( * ) SI_UNIT ( .MILLI., .METRE. ) );
#7894 = CARTESIAN_POINT ( 'NONE',  ( -25.15000000000000213, 0.000000000000000000, 0.000000000000000000 ) ) ;
#7895 = ORIENTED_EDGE ( 'NONE', *, *, #858, .F. ) ;
#7896 = CARTESIAN_POINT ( 'NONE',  ( -16.34436021381890924, 99.50000000000000000, 15.38072013554846151 ) ) ;
#7897 = CARTESIAN_POINT ( 'NONE',  ( -27.43301270000000258, 3.899999998907525800, -11.36312591709336317 ) ) ;
#7898 = ORIENTED_EDGE ( 'NONE', *, *, #6836, .F. ) ;
#7899 = CARTESIAN_POINT ( 'NONE',  ( 2.500000000000000000, -4.274999999999999467, -3.061616997868383141E-16 ) ) ;
#7900 = ITEM_DEFINED_TRANSFORMATION ( 'NONE', 'NONE', #8480,  #5055 ) ;
#7901 = CARTESIAN_POINT ( 'NONE',  ( 3.293841816516395848, 99.99999999999995737, -23.44781013845121009 ) ) ;
#7902 = CARTESIAN_POINT ( 'NONE',  ( -1.595409442497313560E-16, -4.865624999385482319, -2.605501347177161087 ) ) ;
#7903 = CARTESIAN_POINT ( 'NONE',  ( 3.659868213429061878, 99.50000000000000000, -22.50687739797974274 ) ) ;
#7904 = CARTESIAN_POINT ( 'NONE',  ( 1.679787559701184688E-15, 4.549999998907526155, -27.43301270000000258 ) ) ;
#7905 = CIRCLE ( 'NONE', #1712, 0.4999999999999968914 ) ;
#7906 = CARTESIAN_POINT ( 'NONE',  ( 0.000000000000000000, 87.00000000000001421, 0.000000000000000000 ) ) ;
#7907 = CARTESIAN_POINT ( 'NONE',  ( 3.349514647153394975, 99.49999999999998579, -23.95461210612682024 ) ) ;
#7908 = CARTESIAN_POINT ( 'NONE',  ( 3.497829868842083023, 99.50000000000000000, -21.50512556757917793 ) ) ;
#7909 = CARTESIAN_POINT ( 'NONE',  ( 23.82500000000000284, 2.917720998968569322E-15, 0.000000000000000000 ) ) ;
#7910 = CARTESIAN_POINT ( 'NONE',  ( -1.128215178125000273, -3.815624999385482941, -1.954126010382871259 ) ) ;
#7911 = CARTESIAN_POINT ( 'NONE',  ( -21.20585021321354802, 99.50000000000005684, -9.381045134209834657 ) ) ;
#7912 = ORIENTED_EDGE ( 'NONE', *, *, #8577, .F. ) ;
#7913 = CARTESIAN_POINT ( 'NONE',  ( -2.256430356249999214, -1.453124999385482896, 1.302750673588581876 ) ) ;
#7914 = CARTESIAN_POINT ( 'NONE',  ( 27.43301269999999548, 4.199999998907525622, 11.36312591709337738 ) ) ;
#7915 = CARTESIAN_POINT ( 'NONE',  ( 9.513000527211589841, 99.50000000000000000, 20.35102222961602436 ) ) ;
#7916 = PRESENTATION_LAYER_ASSIGNMENT (  '', '', ( #7077 ) ) ;
#7917 = EDGE_CURVE ( 'NONE', #776, #2013, #4404, .T. ) ;
#7918 = CARTESIAN_POINT ( 'NONE',  ( -11.18376618407356560, 1.050000000000000044, -27.00000000000000355 ) ) ;
#7919 = CARTESIAN_POINT ( 'NONE',  ( 9.502908418173033667, 99.50000000000000000, 20.32929868008965002 ) ) ;
#7920 = VERTEX_POINT ( 'NONE', #6734 ) ;
#7921 = LINE ( 'NONE', #7332, #5315 ) ;
#7922 = CARTESIAN_POINT ( 'NONE',  ( 8.074269155311188939, 99.50000000000001421, 20.56111086218762551 ) ) ;
#7923 = ORIENTED_EDGE ( 'NONE', *, *, #4748, .T. ) ;
#7924 = ORIENTED_EDGE ( 'NONE', *, *, #4198, .F. ) ;
#7925 = CARTESIAN_POINT ( 'NONE',  ( -2.256430356250000102, -5.203124999385482674, 0.000000000000000000 ) ) ;
#7926 = CARTESIAN_POINT ( 'NONE',  ( 27.00000000000000355, 0.000000000000000000, 0.000000000000000000 ) ) ;
#7927 = CARTESIAN_POINT ( 'NONE',  ( 1.679787559701184688E-15, 2.849999998907525534, -27.43301270000000258 ) ) ;
#7928 = CARTESIAN_POINT ( 'NONE',  ( -27.00000000000001421, 2.050000000000000266, 11.18376618407356560 ) ) ;
#7929 = FACE_OUTER_BOUND ( 'NONE', #8740, .T. ) ;
#7930 = CARTESIAN_POINT ( 'NONE',  ( -2.256430356250000102, -2.503124999385482496, 0.000000000000000000 ) ) ;
#7931 = CARTESIAN_POINT ( 'NONE',  ( 0.000000000000000000, 0.000000000000000000, 0.000000000000000000 ) ) ;
#7932 = ADVANCED_FACE ( 'NONE', ( #1038 ), #306, .T. ) ;
#7933 = CARTESIAN_POINT ( 'NONE',  ( -16.63177974700816009, 99.50000000000000000, 16.59747536361813403 ) ) ;
#7934 = DIRECTION ( 'NONE',  ( 0.000000000000000000, 0.000000000000000000, 1.000000000000000000 ) ) ;
#7935 = ADVANCED_FACE ( 'NONE', ( #2712 ), #4020, .T. ) ;
#7936 = CARTESIAN_POINT ( 'NONE',  ( -1.250000000000000222, -3.168749998770965526, -2.165063509461096825 ) ) ;
#7937 = VERTEX_POINT ( 'NONE', #6458 ) ;
#7938 = CARTESIAN_POINT ( 'NONE',  ( 2.500000000000000000, -1.068749998770965881, -3.061616997868383141E-16 ) ) ;
#7939 = CARTESIAN_POINT ( 'NONE',  ( -2.500000000000000000, -3.149999999999999467, 0.000000000000000000 ) ) ;
#7940 = ADVANCED_FACE ( 'NONE', ( #1642 ), #5849, .T. ) ;
#7941 = CARTESIAN_POINT ( 'NONE',  ( 7.500000000000000000, 104.5000000000000142, 1.000000000000000222 ) ) ;
#7942 = CARTESIAN_POINT ( 'NONE',  ( -1.128215178124998497, -3.215624999385482408, 1.954126010382872147 ) ) ;
#7943 = ORIENTED_EDGE ( 'NONE', *, *, #9667, .F. ) ;
#7944 = B_SPLINE_SURFACE_WITH_KNOTS ( 'NONE', 3, 1, ( 
 ( #3758, #3815 ),
 ( #2070, #5384 ),
 ( #1237, #4649 ),
 ( #7840, #10144 ),
 ( #671, #9190 ),
 ( #2980, #6161 ),
 ( #4429, #9359 ),
 ( #1401, #4593 ),
 ( #7615, #456 ),
 ( #7784, #616 ),
 ( #3652, #6998 ),
 ( #10202, #9468 ),
 ( #2298, #724 ),
 ( #10258, #4701 ),
 ( #3088, #3918 ),
 ( #7892, #5494 ),
 ( #6273, #8683 ),
 ( #1506, #210 ),
 ( #5015, #1198 ) ),
 .UNSPECIFIED., .F., .F., .F.,
 ( 4, 1, 1, 1, 1, 1, 1, 1, 1, 1, 1, 1, 1, 1, 1, 1, 4 ),
 ( 2, 2 ),
 ( 0.000000000000000000, 0.07024023345195122559, 0.1375772235014411093, 0.2026681864156774648, 0.2655894380381068620, 0.3279415367477454546, 0.3896445486312665740, 0.4521557380645868096, 0.5154465764363311830, 0.5785479733725392704, 0.6397241484143471046, 0.6996998702489094502, 0.7590513234224176564, 0.8180896689983322423, 0.8773873076253557723, 0.9378402036119877216, 1.000000000000000000 ),
 ( 0.000000000000000000, 1.000000000000000000 ),
 .UNSPECIFIED. ) ;
#7945 = ORIENTED_EDGE ( 'NONE', *, *, #10016, .F. ) ;
#7946 = PLANE ( 'NONE',  #8790 ) ;
#7948 = EDGE_CURVE ( 'NONE', #4835, #10148, #9302, .T. ) ;
#7947 = VECTOR ( 'NONE', #2044, 1000.000000000000000 ) ;
#7949 = CARTESIAN_POINT ( 'NONE',  ( -4.959819536546781389E-15, 2.200000000000000178, 27.00000000000000355 ) ) ;
#7950 = DIRECTION ( 'NONE',  ( 0.000000000000000000, 0.000000000000000000, -1.000000000000000000 ) ) ;
#7951 = CARTESIAN_POINT ( 'NONE',  ( 2.939152317953647500E-15, 70.00000000000000000, -23.99999999999999645 ) ) ;
#7952 = ORIENTED_EDGE ( 'NONE', *, *, #1752, .F. ) ;
#7953 = CARTESIAN_POINT ( 'NONE',  ( 5.302876193624534821E-16, -4.837500000000000355, 2.886751345948128655 ) ) ;
#7954 = CARTESIAN_POINT ( 'NONE',  ( 3.563396934924631942, 100.0000000000000142, -22.47881610735839431 ) ) ;
#7955 = CARTESIAN_POINT ( 'NONE',  ( -2.256430356250000102, -4.303124999385482319, 0.000000000000000000 ) ) ;
#7956 = CARTESIAN_POINT ( 'NONE',  ( -20.93486371557392545, 99.49999999999998579, -10.61231311368802466 ) ) ;
#7957 = CARTESIAN_POINT ( 'NONE',  ( -11.18376618407356560, 1.649999997815050357, -27.00000000000000355 ) ) ;
#7958 = VECTOR ( 'NONE', #1937, 1000.000000000000000 ) ;
#7959 = CARTESIAN_POINT ( 'NONE',  ( -20.63200021313574695, 100.0000000000000000, -10.19493994959453431 ) ) ;
#7960 = CARTESIAN_POINT ( 'NONE',  ( 10.85214315541671759, 100.0000000000000000, 22.51047735782115211 ) ) ;
#7961 = CARTESIAN_POINT ( 'NONE',  ( -16.34021191015031249, 99.50000000000000000, 16.45483272884350967 ) ) ;
#7962 = DIRECTION ( 'NONE',  ( -1.224646799147353207E-16, 1.000000000000000000, 0.000000000000000000 ) ) ;
#7963 = CARTESIAN_POINT ( 'NONE',  ( -2.256430356250000102, -3.778124999385482408, -1.302750673588580321 ) ) ;
#7964 = CARTESIAN_POINT ( 'NONE',  ( -20.82968571475833031, 99.50000000000001421, -9.677916414284339908 ) ) ;
#7965 = ORIENTED_EDGE ( 'NONE', *, *, #874, .T. ) ;
#7966 = ORIENTED_EDGE ( 'NONE', *, *, #6082, .T. ) ;
#7967 = CARTESIAN_POINT ( 'NONE',  ( 2.256430356250000102, -1.265624999385482896, -2.763330213280484622E-16 ) ) ;
#7968 = CARTESIAN_POINT ( 'NONE',  ( -19.39806930854668465, 1.649999998907525356, 19.39806930854667755 ) ) ;
#7969 = FACE_OUTER_BOUND ( 'NONE', #7568, .T. ) ;
#7970 = CARTESIAN_POINT ( 'NONE',  ( 27.00000000000000355, 3.200000000000000178, 0.000000000000000000 ) ) ;
#7971 = CARTESIAN_POINT ( 'NONE',  ( -2.256430356250000102, -0.2531249993854829405, 0.000000000000000000 ) ) ;
#7972 = AXIS2_PLACEMENT_3D ( 'NONE', #9229, #7778, #5255 ) ;
#7973 = CARTESIAN_POINT ( 'NONE',  ( -16.37547766376588854, 99.50000000000000000, 16.41943072543956816 ) ) ;
#7974 = CARTESIAN_POINT ( 'NONE',  ( 8.399337394135656609, 99.99999999999998579, 20.06291166101774692 ) ) ;
#7975 = CYLINDRICAL_SURFACE ( 'NONE', #9824, 2.500000000000000000 ) ;
#7976 = ORIENTED_EDGE ( 'NONE', *, *, #1897, .F. ) ;
#7977 = EDGE_CURVE ( 'NONE', #7639, #6902, #9418, .T. ) ;
#7978 = CARTESIAN_POINT ( 'NONE',  ( 11.36312591709336850, 3.299999998907525711, 27.43301269999999903 ) ) ;
#7979 = CARTESIAN_POINT ( 'NONE',  ( 3.024867170474271116, 99.99999999999995737, -24.05477125543085748 ) ) ;
#7980 = DIRECTION ( 'NONE',  ( -0.8660254037844385966, -0.000000000000000000, -0.5000000000000001110 ) ) ;
#7981 = VECTOR ( 'NONE', #5698, 1000.000000000000000 ) ;
#7982=STYLED_ITEM('',(#10394),#6298);
#7983 = CARTESIAN_POINT ( 'NONE',  ( -2.256430356250000102, -3.403124999385482408, 0.000000000000000000 ) ) ;
#7984 = CARTESIAN_POINT ( 'NONE',  ( 0.000000000000000000, -5.000000000000000000, 0.000000000000000000 ) ) ;
#7985 = CARTESIAN_POINT ( 'NONE',  ( 1.653273178848927064E-15, 1.800000000000000266, -27.00000000000000355 ) ) ;
#7986 = CARTESIAN_POINT ( 'NONE',  ( 19.09188309203678813, 5.499999997815050001, -19.09188309203678813 ) ) ;
#7987 = B_SPLINE_CURVE_WITH_KNOTS ( 'NONE', 3,
 ( #2816, #6049, #2982, #6163, #9361, #3038, #1293, #5387, #8579, #9239, #4595, #2072, #6217, #5267, #9414, #8465, #4024, #5495, #2300 ),
 .UNSPECIFIED., .F., .F.,
 ( 4, 1, 1, 1, 1, 1, 1, 1, 1, 1, 1, 1, 1, 1, 1, 1, 4 ),
 ( 0.000000000000000000, 0.06442465027149940626, 0.1272622498775801414, 0.1890519169419207224, 0.2498421757728049863, 0.3110425729590077792, 0.3720985300252119266, 0.4351465435385043490, 0.5001170788027262670, 0.5644817420234762295, 0.6276143074669133792, 0.6889588046791949028, 0.7501592018653976401, 0.8106582772613761811, 0.8724479443257179279, 0.9351683423010851426, 1.000000000000000000 ),
 .UNSPECIFIED. ) ;
#7988 = CARTESIAN_POINT ( 'NONE',  ( 1.250000000000001110, -2.943749998770965437, 2.165063509461096380 ) ) ;
#7989 = VERTEX_POINT ( 'NONE', #8583 ) ;
#7990 = EDGE_CURVE ( 'NONE', #7824, #6922, #7845, .T. ) ;
#7991 = CARTESIAN_POINT ( 'NONE',  ( 2.939152317953647500E-15, 70.00000000000000000, -23.99999999999999645 ) ) ;
#7992 = CARTESIAN_POINT ( 'NONE',  ( 0.000000000000000000, 0.000000000000000000, 0.000000000000000000 ) ) ;
#7993 = CARTESIAN_POINT ( 'NONE',  ( -22.24883010645271852, 99.49999999999997158, -10.75389422444101939 ) ) ;
#7994 = CARTESIAN_POINT ( 'NONE',  ( -1.595409442497313560E-16, -2.953124999385482674, -2.605501347177161087 ) ) ;
#7995 = ORIENTED_EDGE ( 'NONE', *, *, #3140, .F. ) ;
#7996 = CARTESIAN_POINT ( 'NONE',  ( 3.000000000000000000, -15.00000000000000000, -1.732050807568876749 ) ) ;
#7997 = AXIS2_PLACEMENT_3D ( 'NONE', #8797, #3985, #107 ) ;
#7998 = SURFACE_SIDE_STYLE ('',( #4803 ) ) ;
#7999 = CARTESIAN_POINT ( 'NONE',  ( 0.6698729810778075722, -2.061153809338631238, 2.499999999999999556 ) ) ;
#8000 = LINE ( 'NONE', #5648, #7981 ) ;
#8001 = CARTESIAN_POINT ( 'NONE',  ( 11.36312591709336139, 4.499999998907525445, -27.43301270000000258 ) ) ;
#8002 = VERTEX_POINT ( 'NONE', #10032 ) ;
#8003 = AXIS2_PLACEMENT_3D ( 'NONE', #6946, #7788, #2866 ) ;
#8004 = CARTESIAN_POINT ( 'NONE',  ( -2.500000000000000000, -4.049999999999999822, 0.000000000000000000 ) ) ;
#8005 = CARTESIAN_POINT ( 'NONE',  ( -21.28703419482447146, 99.99999999999997158, -11.01737971290317297 ) ) ;
#8006 =( BOUNDED_CURVE ( )  B_SPLINE_CURVE ( 2, ( #8048, #4073, #1510, #7255, #2302, #980, #6616, #7353, #9760 ),
 .UNSPECIFIED., .F., .T. ) 
 B_SPLINE_CURVE_WITH_KNOTS ( ( 3, 2, 2, 2, 3 ),
 ( 0.3214285714285714524, 0.3392857142857143016, 0.3571428571428571508, 0.3750000000000000000, 0.3928571428571428492 ),
 .UNSPECIFIED. ) 
 CURVE ( )  GEOMETRIC_REPRESENTATION_ITEM ( )  RATIONAL_B_SPLINE_CURVE ( ( 1.000000000000000000, 0.9238795325112867385, 1.000000000000000000, 0.9238795325112867385, 1.000000000000000000, 0.9238795325112867385, 1.000000000000000000, 0.9238795325112867385, 1.000000000000000000 ) ) 
 REPRESENTATION_ITEM ( '' )  );
#8007 = CARTESIAN_POINT ( 'NONE',  ( 2.256430356250000546, -3.665624999385482141, 1.302750673588579877 ) ) ;
#8008 = CARTESIAN_POINT ( 'NONE',  ( -21.16695614262292580, 100.0000000000000000, -11.33496398805607441 ) ) ;
#8009 = CARTESIAN_POINT ( 'NONE',  ( 26.99999999999999645, 2.149999997815051245, 11.18376618407358691 ) ) ;
#8010 = UNCERTAINTY_MEASURE_WITH_UNIT (LENGTH_MEASURE( 1.000000000000000082E-05 ), #1005, 'distance_accuracy_value', 'NONE');
#8011 = B_SPLINE_CURVE_WITH_KNOTS ( 'NONE', 3,
 ( #9895, #2931, #5823, #2731, #174, #6057, #1058, #9013, #9248, #5275, #8968, #6113, #7431, #272, #3464, #8474, #4492, #2678, #6653 ),
 .UNSPECIFIED., .F., .F.,
 ( 4, 1, 1, 1, 1, 1, 1, 1, 1, 1, 1, 1, 1, 1, 1, 1, 4 ),
 ( 0.000000000000000000, 0.06222907146265880401, 0.1227741760084055250, 0.1821991178386986321, 0.2415152369242211383, 0.3014228132391471027, 0.3622599083280184651, 0.4248173832850619669, 0.4890434280230284148, 0.5537961591902206271, 0.6173286602167864512, 0.6798064121185800612, 0.7417947397634444551, 0.8039614856828293243, 0.8674939867093949264, 0.9325113003366737319, 1.000000000000000000 ),
 .UNSPECIFIED. ) ;
#8012 = CARTESIAN_POINT ( 'NONE',  ( -20.66709314808276332, 99.50000000000002842, -10.01107456535036455 ) ) ;
#8013 = LINE ( 'NONE', #2464, #3822 ) ;
#8014 = CARTESIAN_POINT ( 'NONE',  ( 0.000000000000000000, 5.000000000000000000, -27.00000000000000000 ) ) ;
#8015 = ADVANCED_FACE ( 'NONE', ( #6165 ), #3762, .F. ) ;
#8016 = CARTESIAN_POINT ( 'NONE',  ( -22.13144646319157260, 100.0000000000000142, -9.428651666388001118 ) ) ;
#8017 = CARTESIAN_POINT ( 'NONE',  ( -1.128215178125000273, -2.915624999385482585, -1.954126010382871259 ) ) ;
#8018 = CARTESIAN_POINT ( 'NONE',  ( 0.6698729810778063509, -2.382596189432333755, -2.500000000000000000 ) ) ;
#8019 = ORIENTED_EDGE ( 'NONE', *, *, #5442, .T. ) ;
#8020 = CARTESIAN_POINT ( 'NONE',  ( 4.786228327491941173E-16, -1.828124999385482896, 2.605501347177161087 ) ) ;
#8021 = CARTESIAN_POINT ( 'NONE',  ( -27.43301270000000258, 1.499999998907525223, -11.36312591709336317 ) ) ;
#8022 =( NAMED_UNIT ( * ) SI_UNIT ( $, .STERADIAN. ) SOLID_ANGLE_UNIT ( ) );
#8023 = DIRECTION ( 'NONE',  ( 0.000000000000000000, 0.000000000000000000, -1.000000000000000000 ) ) ;
#8024 = CARTESIAN_POINT ( 'NONE',  ( 27.00000000000000355, 4.049999999999999822, -11.18376618407356737 ) ) ;
#8025 = DIRECTION ( 'NONE',  ( 0.000000000000000000, 0.000000000000000000, -1.000000000000000000 ) ) ;
#8026 = DIRECTION ( 'NONE',  ( 0.000000000000000000, 1.000000000000000000, -0.000000000000000000 ) ) ;
#8027 = DIRECTION ( 'NONE',  ( -0.000000000000000000, 1.000000000000000000, -0.000000000000000000 ) ) ;
#8028 = CARTESIAN_POINT ( 'NONE',  ( 6.477538756577482459, 99.50000000000000000, 20.49684993083915430 ) ) ;
#8029 = VERTEX_POINT ( 'NONE', #6002 ) ;
#8030 = CARTESIAN_POINT ( 'NONE',  ( -19.39806930854668465, 3.949999998907525178, 19.39806930854667755 ) ) ;
#8031 = CARTESIAN_POINT ( 'NONE',  ( 2.500000000000000000, -4.181249998770965703, -1.443375672974065438 ) ) ;
#8032 = PRODUCT_DEFINITION_SHAPE ( 'NONE', 'NONE',  #10369 ) ;
#8033 = CARTESIAN_POINT ( 'NONE',  ( -22.57971655928959365, 100.0000000000000000, -10.84768434062017839 ) ) ;
#8034 = CARTESIAN_POINT ( 'NONE',  ( -2.256430356249998770, -4.715624999385481964, 1.302750673588581876 ) ) ;
#8035 = CARTESIAN_POINT ( 'NONE',  ( -16.41302370085497131, 99.99999999999998579, 15.45185748370271206 ) ) ;
#8036 = CARTESIAN_POINT ( 'NONE',  ( -16.91659681606879317, 99.50000000000000000, 15.78485274883190392 ) ) ;
#8037 = CARTESIAN_POINT ( 'NONE',  ( 8.122452352567329115, 100.0000000000000000, 21.04970292111833530 ) ) ;
#8038 = CARTESIAN_POINT ( 'NONE',  ( 1.249999999999999334, -2.343749998770965792, -2.165063509461096825 ) ) ;
#8039 = AXIS2_PLACEMENT_3D ( 'NONE', #1292, #6833, #8520 ) ;
#8040 = CARTESIAN_POINT ( 'NONE',  ( 4.280752963211088336, 99.99999999999997158, -21.16602454745684270 ) ) ;
#8041 = CARTESIAN_POINT ( 'NONE',  ( -20.64578974631102426, 99.49999999999995737, -10.10077944494247504 ) ) ;
#8042 = CARTESIAN_POINT ( 'NONE',  ( 9.725694684612619767, 99.50000000000000000, 20.03234812723199454 ) ) ;
#8043 = CARTESIAN_POINT ( 'NONE',  ( 2.256430356249999658, -3.028124999385482852, -1.302750673588581432 ) ) ;
#8044 = B_SPLINE_CURVE_WITH_KNOTS ( 'NONE', 3,
 ( #4922, #8710, #8755, #3260, #6398, #6449, #1579, #8857, #4143, #162, #902 ),
 .UNSPECIFIED., .F., .F.,
 ( 4, 1, 1, 1, 1, 1, 1, 1, 4 ),
 ( 0.000000000000000000, 0.09809051273808343241, 0.1997563395654988194, 0.3058527769869914259, 0.4162847437678430240, 0.5377099880548563693, 0.6743560419832976827, 0.8289895874771281425, 1.000000000000000000 ),
 .UNSPECIFIED. ) ;
#8045 = EDGE_CURVE ( 'NONE', #2404, #2471, #2969, .T. ) ;
#8046 = CARTESIAN_POINT ( 'NONE',  ( 0.000000000000000000, 70.00000000000000000, 0.000000000000000000 ) ) ;
#8047 = CARTESIAN_POINT ( 'NONE',  ( -22.33391032228853490, 99.50000000000002842, -10.55243757774135993 ) ) ;
#8048 = CARTESIAN_POINT ( 'NONE',  ( 1.653273178848927064E-15, 2.399999997815050357, -27.00000000000000355 ) ) ;
#8049 = CARTESIAN_POINT ( 'NONE',  ( 9.513000527211589841, 100.0000000000000000, 20.35102222961602436 ) ) ;
#8050 = VERTEX_POINT ( 'NONE', #9363 ) ;
#8051 = CARTESIAN_POINT ( 'NONE',  ( 0.000000000000000000, 97.50000000000000000, 0.000000000000000000 ) ) ;
#8052 =( GEOMETRIC_REPRESENTATION_CONTEXT ( 3 ) GLOBAL_UNCERTAINTY_ASSIGNED_CONTEXT ( ( #4444 ) ) GLOBAL_UNIT_ASSIGNED_CONTEXT ( ( #459, #7409, #1086 ) ) REPRESENTATION_CONTEXT ( 'NONE', 'WORKASPACE' ) );
#8053 = CARTESIAN_POINT ( 'NONE',  ( 2.837666006185522782, 99.99999999999997158, -22.03040394835428373 ) ) ;
#8054 = CARTESIAN_POINT ( 'NONE',  ( 2.256430356250000546, -3.215624999385482408, 1.302750673588579877 ) ) ;
#8055 = ADVANCED_FACE ( 'NONE', ( #7620 ), #5529, .T. ) ;
#8056 = CARTESIAN_POINT ( 'NONE',  ( 4.100286767325537873, 99.50000000000000000, -22.51382885696750336 ) ) ;
#8057 = CARTESIAN_POINT ( 'NONE',  ( 11.18376618407356915, 2.349999997815050090, -27.00000000000000355 ) ) ;
#8058 = CARTESIAN_POINT ( 'NONE',  ( -15.31787750341841559, 99.50000000000000000, 16.43551622900274722 ) ) ;
#8059 = CARTESIAN_POINT ( 'NONE',  ( -21.94169572595625795, 99.50000000000000000, -9.715372641902229489 ) ) ;
#8060 = CYLINDRICAL_SURFACE ( 'NONE', #6406, 2.500000000000000000 ) ;
#8061 = VECTOR ( 'NONE', #7242, 1000.000000000000000 ) ;
#8062 = CARTESIAN_POINT ( 'NONE',  ( -22.63784607493503387, 100.0000000000000142, -10.71517552924587058 ) ) ;
#8063 = CARTESIAN_POINT ( 'NONE',  ( -1.128215178125000273, -3.365624999385482763, -1.954126010382871259 ) ) ;
#8064 = CARTESIAN_POINT ( 'NONE',  ( 9.583828860305853681, 99.99999999999998579, 20.68614437522342797 ) ) ;
#8065 = PRODUCT_RELATED_PRODUCT_CATEGORY ( 'part', '', ( #7772 ) ) ;
#8066 = EDGE_LOOP ( 'NONE', ( #9194, #1855, #460, #3236, #4928, #9971 ) ) ;
#8067 = CARTESIAN_POINT ( 'NONE',  ( 4.786228327491941173E-16, -3.628124999385482941, 2.605501347177161087 ) ) ;
#8068 =( BOUNDED_CURVE ( )  B_SPLINE_CURVE ( 2, ( #6275, #10361, #3192, #8785, #6479, #1610, #4804, #7999, #9668 ),
 .UNSPECIFIED., .F., .F. ) 
 B_SPLINE_CURVE_WITH_KNOTS ( ( 3, 2, 2, 2, 3 ),
 ( 0.2708333333333333703, 0.2777777777777777901, 0.2916666666666666852, 0.3055555555555555802, 0.3125000000000000000 ),
 .UNSPECIFIED. ) 
 CURVE ( )  GEOMETRIC_REPRESENTATION_ITEM ( )  RATIONAL_B_SPLINE_CURVE ( ( 0.9330127018922194093, 0.9330127018922196314, 1.000000000000000000, 0.8660254037844387076, 1.000000000000000000, 0.8660254037844387076, 1.000000000000000000, 0.9330127018922194093, 0.9330127018922194093 ) ) 
 REPRESENTATION_ITEM ( '' )  );
#8069 = CARTESIAN_POINT ( 'NONE',  ( 1.679787559701184688E-15, 2.149999998907525356, -27.43301270000000258 ) ) ;
#8070 = ADVANCED_FACE ( 'NONE', ( #3819 ), #4501, .T. ) ;
#8071 = PRESENTATION_STYLE_ASSIGNMENT (( #3995 ) ) ;
#8072 = DIRECTION ( 'NONE',  ( 0.000000000000000000, 0.000000000000000000, -1.000000000000000000 ) ) ;
#8073 = AXIS2_PLACEMENT_3D ( 'NONE', #10179, #4628, #5473 ) ;
#8074 = EDGE_CURVE ( 'NONE', #5471, #4614, #8000, .T. ) ;
#8075 = CARTESIAN_POINT ( 'NONE',  ( 27.00000000000000355, 4.000000000000000000, 0.000000000000000000 ) ) ;
#8076 = CARTESIAN_POINT ( 'NONE',  ( -20.88772068548257366, 100.0000000000000142, -11.14739719174079546 ) ) ;
#8077 = ORIENTED_EDGE ( 'NONE', *, *, #6253, .T. ) ;
#8078 = DIRECTION ( 'NONE',  ( 0.000000000000000000, 0.000000000000000000, -1.000000000000000000 ) ) ;
#8079 = CARTESIAN_POINT ( 'NONE',  ( 0.000000000000000000, 100.0000000000000000, 0.000000000000000000 ) ) ;
#8080 = ORIENTED_EDGE ( 'NONE', *, *, #2037, .F. ) ;
#8081 = CIRCLE ( 'NONE', #3553, 25.15000000000000213 ) ;
#8082 = CARTESIAN_POINT ( 'NONE',  ( 27.43301269999999548, 3.399999998907525356, 11.36312591709337916 ) ) ;
#8083 = AXIS2_PLACEMENT_3D ( 'NONE', #7503, #1126, #504 ) ;
#8084 = CARTESIAN_POINT ( 'NONE',  ( 3.293272160652527258, 99.49999999999997158, -24.41359064397622802 ) ) ;
#8085 = CARTESIAN_POINT ( 'NONE',  ( -22.43115009631934953, 100.0000000000000142, -11.08196351649073819 ) ) ;
#8086 = CARTESIAN_POINT ( 'NONE',  ( -1.595409442497313560E-16, -4.865624999385482319, -2.605501347177161087 ) ) ;
#8087 = CARTESIAN_POINT ( 'NONE',  ( -19.09188309203678457, 1.699999997815050401, -19.09188309203678813 ) ) ;
#8088 = CARTESIAN_POINT ( 'NONE',  ( -16.74216497804568604, 99.50000000000001421, 15.31795814478965312 ) ) ;
#8089 = CARTESIAN_POINT ( 'NONE',  ( 8.063732359723156051, 100.0000000000000142, 20.72384750152746236 ) ) ;
#8090 = VECTOR ( 'NONE', #1277, 1000.000000000000000 ) ;
#8091 = CARTESIAN_POINT ( 'NONE',  ( -1.250000000000000222, -4.068749998770965881, -2.165063509461096825 ) ) ;
#8092 = ORIENTED_EDGE ( 'NONE', *, *, #7781, .T. ) ;
#8093 = EDGE_LOOP ( 'NONE', ( #6713, #10264, #2286, #5291 ) ) ;
#8094 = CARTESIAN_POINT ( 'NONE',  ( -22.33391032228853490, 99.50000000000002842, -10.55243757774135993 ) ) ;
#8095 = CARTESIAN_POINT ( 'NONE',  ( -3.061616997868383634E-16, -20.00000000000000000, 2.500000000000000444 ) ) ;
#8096 = DIRECTION ( 'NONE',  ( -0.2149789550291109352, 0.000000000000000000, -0.9766186814179788067 ) ) ;
#8097 = CARTESIAN_POINT ( 'NONE',  ( 2.256430356250000102, -3.965624999385482408, -2.763330213280484622E-16 ) ) ;
#8098 = LINE ( 'NONE', #3477, #10154 ) ;
#8099 = LINE ( 'NONE', #5835, #2999 ) ;
#8100 = EDGE_CURVE ( 'NONE', #5685, #4986, #4806, .T. ) ;
#8101 = CARTESIAN_POINT ( 'NONE',  ( -16.25072943800822500, 99.50000000000005684, 15.30228603765648820 ) ) ;
#8102 = CARTESIAN_POINT ( 'NONE',  ( -27.00000000000000355, 4.350000000000000533, -11.18376618407357270 ) ) ;
#8103 = ORIENTED_EDGE ( 'NONE', *, *, #8630, .T. ) ;
#8104 = ADVANCED_FACE ( 'NONE', ( #2347 ), #7308, .T. ) ;
#8105 = CARTESIAN_POINT ( 'NONE',  ( 4.232447118646125439, 99.49999999999998579, -21.54138831197867887 ) ) ;
#8106 = AXIS2_PLACEMENT_3D ( 'NONE', #10055, #5468, #3733 ) ;
#8107 = CARTESIAN_POINT ( 'NONE',  ( -21.24310748994415832, 99.99999999999998579, -10.99527971241054658 ) ) ;
#8108 = CARTESIAN_POINT ( 'NONE',  ( 2.256430356249999658, -0.3281249993854829516, -1.302750673588581432 ) ) ;
#8109 = CARTESIAN_POINT ( 'NONE',  ( -20.42657152723830905, 100.0000000000000000, -10.54129411626120216 ) ) ;
#8110 = CARTESIAN_POINT ( 'NONE',  ( 11.36312591709336850, 4.199999998907525622, 27.43301269999999903 ) ) ;
#8111 = FACE_OUTER_BOUND ( 'NONE', #4418, .T. ) ;
#8112 = CARTESIAN_POINT ( 'NONE',  ( 27.00000000000000355, 3.799999997815050268, 0.000000000000000000 ) ) ;
#8113 = CARTESIAN_POINT ( 'NONE',  ( 3.446946945638383664, 99.99999999999997158, -21.53774374131874580 ) ) ;
#8114 = DIRECTION ( 'NONE',  ( 6.944978907077980968E-14, -1.000000000000000000, -3.537534599156363020E-12 ) ) ;
#8115 = CARTESIAN_POINT ( 'NONE',  ( 4.786228327491940187E-16, -3.628124999385482941, 2.605501347177161087 ) ) ;
#8116 = EDGE_CURVE ( 'NONE', #3729, #393, #1710, .T. ) ;
#8117 = CARTESIAN_POINT ( 'NONE',  ( -1.214319963873739860, -5.167334288697576383, -2.063219373018434943 ) ) ;
#8118 = CARTESIAN_POINT ( 'NONE',  ( 0.000000000000000000, 0.000000000000000000, 0.000000000000000000 ) ) ;
#8119 = DIRECTION ( 'NONE',  ( 0.000000000000000000, 0.000000000000000000, -1.000000000000000000 ) ) ;
#8120 = CARTESIAN_POINT ( 'NONE',  ( -27.43301270000000969, 0.6999999989075252893, 11.36312591709335429 ) ) ;
#8121 = DIRECTION ( 'NONE',  ( 0.000000000000000000, -1.000000000000000000, 0.000000000000000000 ) ) ;
#8122 = EDGE_CURVE ( 'NONE', #1073, #2960, #163, .T. ) ;
#8123 = FACE_OUTER_BOUND ( 'NONE', #4375, .T. ) ;
#8124 = PRESENTATION_STYLE_ASSIGNMENT (( #1585 ) ) ;
#8125 = CARTESIAN_POINT ( 'NONE',  ( -21.30928386698190025, 99.50000000000000000, -11.02857376369709996 ) ) ;
#8126 = ADVANCED_FACE ( 'NONE', ( #2401 ), #1611, .T. ) ;
#8127 = CIRCLE ( 'NONE', #8795, 30.00000000000000000 ) ;
#8128 =( BOUNDED_CURVE ( )  B_SPLINE_CURVE ( 2, ( #709, #1335, #6257, #1443, #8672, #7876, #2967, #3690, #552 ),
 .UNSPECIFIED., .F., .F. ) 
 B_SPLINE_CURVE_WITH_KNOTS ( ( 3, 2, 2, 2, 3 ),
 ( 0.6071428571428570953, 0.6250000000000000000, 0.6428571428571429047, 0.6607142857142856984, 0.6785714285714286031 ),
 .UNSPECIFIED. ) 
 CURVE ( )  GEOMETRIC_REPRESENTATION_ITEM ( )  RATIONAL_B_SPLINE_CURVE ( ( 1.000000000000000000, 0.9238795325112867385, 1.000000000000000000, 0.9238795325112867385, 1.000000000000000000, 0.9238795325112867385, 1.000000000000000000, 0.9238795325112867385, 1.000000000000000000 ) ) 
 REPRESENTATION_ITEM ( '' )  );
#8129 = ORIENTED_EDGE ( 'NONE', *, *, #9605, .T. ) ;
#8130 = DIRECTION ( 'NONE',  ( 0.000000000000000000, -1.000000000000000000, 0.000000000000000000 ) ) ;
#8131 = CARTESIAN_POINT ( 'NONE',  ( 3.171774962637509798, 100.0000000000000000, -24.28498992023182268 ) ) ;
#8132 = FILL_AREA_STYLE ('',( #4934 ) ) ;
#8133 = CARTESIAN_POINT ( 'NONE',  ( 1.128215178124999607, -4.453124999385482674, -1.954126010382871259 ) ) ;
#8134 = DIRECTION ( 'NONE',  ( 0.000000000000000000, 0.000000000000000000, 1.000000000000000000 ) ) ;
#8135 = CARTESIAN_POINT ( 'NONE',  ( -22.69331084068295112, 99.49999999999998579, -10.43328931840349050 ) ) ;
#8136 = AXIS2_PLACEMENT_3D ( 'NONE', #2589, #4941, #9802 ) ;
#8137 = FACE_OUTER_BOUND ( 'NONE', #3392, .T. ) ;
#8138 = CARTESIAN_POINT ( 'NONE',  ( -2.500000000000000000, -3.543749998770965526, 0.000000000000000000 ) ) ;
#8139 = ORIENTED_EDGE ( 'NONE', *, *, #5765, .F. ) ;
#8140 = ORIENTED_EDGE ( 'NONE', *, *, #4682, .T. ) ;
#8141 = EDGE_CURVE ( 'NONE', #9715, #9319, #6974, .T. ) ;
#8142 = CIRCLE ( 'NONE', #1108, 27.00000000000000355 ) ;
#8143 = CARTESIAN_POINT ( 'NONE',  ( -22.29247428061501779, 99.50000000000000000, -10.66603791136541624 ) ) ;
#8144 = CARTESIAN_POINT ( 'NONE',  ( -18.01369080470046313, 100.0000000000000000, 17.15556831233607937 ) ) ;
#8145 = CARTESIAN_POINT ( 'NONE',  ( -21.44539290152690114, 99.50000000000000000, -11.08070480119962298 ) ) ;
#8146 = CARTESIAN_POINT ( 'NONE',  ( 2.256430356250000546, -4.903124999385481964, 1.302750673588579877 ) ) ;
#8147 = AXIS2_PLACEMENT_3D ( 'NONE', #2578, #7136, #8718 ) ;
#8148 = PRESENTATION_LAYER_ASSIGNMENT (  '', '', ( #1947 ) ) ;
#8149 = EDGE_LOOP ( 'NONE', ( #454, #8362, #8183, #5238 ) ) ;
#8150 = CARTESIAN_POINT ( 'NONE',  ( 8.187169943530866689, 99.49999999999998579, 20.27434297626003712 ) ) ;
#8151 = CARTESIAN_POINT ( 'NONE',  ( 21.47055288461538325, 99.50000000000000000, -0.7081330128205128860 ) ) ;
#8152 = CARTESIAN_POINT ( 'NONE',  ( 0.000000000000000000, 100.0000000000000000, -25.15000000000000213 ) ) ;
#8153 = CARTESIAN_POINT ( 'NONE',  ( 3.375079225685456041, 100.0000000000000000, -22.79123997459842954 ) ) ;
#8154 = CARTESIAN_POINT ( 'NONE',  ( 4.241330131419338123, 99.49999999999998579, -24.68798891778770965 ) ) ;
#8155 = CARTESIAN_POINT ( 'NONE',  ( 4.277141017070624329, 99.50000000000002842, -21.57940364907851816 ) ) ;
#8156 = PLANE ( 'NONE',  #2274 ) ;
#8157 = CARTESIAN_POINT ( 'NONE',  ( 19.09188309203678813, 5.499999997815050001, -19.09188309203678813 ) ) ;
#8158 = PLANE ( 'NONE',  #4777 ) ;
#8159 = CARTESIAN_POINT ( 'NONE',  ( 0.000000000000000000, 0.000000000000000000, 0.000000000000000000 ) ) ;
#8160 = FACE_OUTER_BOUND ( 'NONE', #2693, .T. ) ;
#8161 = VECTOR ( 'NONE', #1675, 1000.000000000000000 ) ;
#8162 = ORIENTED_EDGE ( 'NONE', *, *, #3465, .F. ) ;
#8163 = CARTESIAN_POINT ( 'NONE',  ( 2.256430356250000102, -4.415624999385482141, -2.763330213280484622E-16 ) ) ;
#8164 = CARTESIAN_POINT ( 'NONE',  ( -15.07178375341841381, 99.99999999999998579, 16.66969090848992607 ) ) ;
#8165 = CARTESIAN_POINT ( 'NONE',  ( 0.000000000000000000, 97.50000000000000000, 18.00000000000000000 ) ) ;
#8166 = CARTESIAN_POINT ( 'NONE',  ( 1.653273178848927064E-15, 5.000000000000000000, -27.00000000000000355 ) ) ;
#8167 = CARTESIAN_POINT ( 'NONE',  ( 21.82251602564102910, 100.0000000000000000, -0.5181290064102563875 ) ) ;
#8168 = B_SPLINE_CURVE_WITH_KNOTS ( 'NONE', 3,
 ( #9921, #2755, #6529, #5794, #1853, #4222, #8938, #5947, #1130, #1806, #9138, #7506, #1958, #244, #5153, #4953, #8351, #8154, #3428 ),
 .UNSPECIFIED., .F., .F.,
 ( 4, 1, 1, 1, 1, 1, 1, 1, 1, 1, 1, 1, 1, 1, 1, 1, 4 ),
 ( 0.000000000000000000, 0.08029080299619884009, 0.1602734547033792534, 0.2412010114815648643, 0.3246404098231062685, 0.3670482715230247162, 0.4085690013065461645, 0.4496707568484641926, 0.4905395156191099670, 0.5313644394553277417, 0.5726744073239632415, 0.6138178896263115636, 0.6555018086025313773, 0.7394546411270094266, 0.8240219501092651555, 0.9101625766452680066, 1.000000000000000000 ),
 .UNSPECIFIED. ) ;
#8169 = EDGE_CURVE ( 'NONE', #7890, #5137, #1238, .T. ) ;
#8170 = CARTESIAN_POINT ( 'NONE',  ( -2.500000000000000000, -1.387499999999999734, -1.443375672974064106 ) ) ;
#8171 = LINE ( 'NONE', #1203, #6149 ) ;
#8172 = CARTESIAN_POINT ( 'NONE',  ( -20.99557965837879081, 99.49999999999997158, -10.74478602187354959 ) ) ;
#8173 = ORIENTED_EDGE ( 'NONE', *, *, #2031, .T. ) ;
#8174 = CARTESIAN_POINT ( 'NONE',  ( -21.30033281797529909, 99.99999999999995737, -9.345151174687854834 ) ) ;
#8175 = CARTESIAN_POINT ( 'NONE',  ( 0.000000000000000000, 87.00000000000001421, -24.00000000000000355 ) ) ;
#8176 = CARTESIAN_POINT ( 'NONE',  ( 27.43301270000000258, 0.2999999989075252671, -11.36312591709336139 ) ) ;
#8177 = SURFACE_SIDE_STYLE ('',( #961 ) ) ;
#8178 = CARTESIAN_POINT ( 'NONE',  ( 2.256430356249999658, -3.590624999385482408, -1.302750673588581432 ) ) ;
#8179 = CARTESIAN_POINT ( 'NONE',  ( -22.21668755910108928, 99.50000000000004263, -9.472979539922778969 ) ) ;
#8180 = CARTESIAN_POINT ( 'NONE',  ( -16.79604063091391097, 100.0000000000000000, 15.40463673182947701 ) ) ;
#8181 = ORIENTED_EDGE ( 'NONE', *, *, #3637, .T. ) ;
#8182 = CARTESIAN_POINT ( 'NONE',  ( 5.179363668139080445, 100.0000000000000711, -23.94265746362379943 ) ) ;
#8183 = ORIENTED_EDGE ( 'NONE', *, *, #3389, .T. ) ;
#8184 = CARTESIAN_POINT ( 'NONE',  ( -1.128215178125000273, -0.3281249993854828961, -1.954126010382871259 ) ) ;
#8185 = EDGE_LOOP ( 'NONE', ( #3112, #3968, #2605, #3032 ) ) ;
#8186 = ORIENTED_EDGE ( 'NONE', *, *, #4844, .T. ) ;
#8187 = CARTESIAN_POINT ( 'NONE',  ( -22.43115009631934953, 100.0000000000000142, -11.08196351649073819 ) ) ;
#8188 = CARTESIAN_POINT ( 'NONE',  ( 3.202955020264580899, 99.99999999999997158, -21.91595956354277064 ) ) ;
#8189 = CARTESIAN_POINT ( 'NONE',  ( -22.20893716642541804, 99.50000000000002842, -10.81429252070940272 ) ) ;
#8190 = CARTESIAN_POINT ( 'NONE',  ( -15.10382517959271098, 99.99999999999998579, 15.91526905993627317 ) ) ;
#8191 = EDGE_CURVE ( 'NONE', #8491, #7890, #8006, .T. ) ;
#8192 = ADVANCED_FACE ( 'NONE', ( #1802 ), #7499, .F. ) ;
#8193 = CARTESIAN_POINT ( 'NONE',  ( 2.500000000000000000, -1.537500000000000089, -1.443375672974065438 ) ) ;
#8194 = FACE_BOUND ( 'NONE', #6549, .T. ) ;
#8195 = CARTESIAN_POINT ( 'NONE',  ( -21.93524539549613550, 99.99999999999998579, -11.03420246938663318 ) ) ;
#8196 = ORIENTED_EDGE ( 'NONE', *, *, #8116, .F. ) ;
#8197 = CARTESIAN_POINT ( 'NONE',  ( 3.124251205490514494, 100.0000000000000000, -23.02140944421609703 ) ) ;
#8198 = CARTESIAN_POINT ( 'NONE',  ( 3.817429849879703241, 99.49999999999998579, -22.92346308580664171 ) ) ;
#8199 = CARTESIAN_POINT ( 'NONE',  ( 4.049441352997683374, 99.50000000000000000, -21.43849541167161732 ) ) ;
#8200 = ORIENTED_EDGE ( 'NONE', *, *, #10192, .T. ) ;
#8201 = CARTESIAN_POINT ( 'NONE',  ( 3.212364564527730337, 100.0000000000000284, -22.10366694310577884 ) ) ;
#8202 = CARTESIAN_POINT ( 'NONE',  ( -27.00000000000000355, 4.149999997815050357, -11.18376618407357093 ) ) ;
#8203 = FACE_OUTER_BOUND ( 'NONE', #4920, .T. ) ;
#8204 = CARTESIAN_POINT ( 'NONE',  ( -21.66466628782423243, 99.50000000000001421, -9.640935998098070669 ) ) ;
#8205 = CARTESIAN_POINT ( 'NONE',  ( -22.27115127098604574, 99.50000000000000000, -10.71048520281369676 ) ) ;
#8206 = CARTESIAN_POINT ( 'NONE',  ( 3.681717055787076642, 100.0000000000000000, -21.09125273517263111 ) ) ;
#8207 = CARTESIAN_POINT ( 'NONE',  ( -2.500000000000000000, -2.250000000000000000, 0.000000000000000000 ) ) ;
#8208 = VERTEX_POINT ( 'NONE', #3334 ) ;
#8209 = CARTESIAN_POINT ( 'NONE',  ( 2.256430356250000546, -3.553124999385482763, 1.302750673588579877 ) ) ;
#8210 = SURFACE_SIDE_STYLE ('',( #4964 ) ) ;
#8211 = CARTESIAN_POINT ( 'NONE',  ( -15.03933290382598820, 99.99999999999998579, 15.19633946010233849 ) ) ;
#8212 = LINE ( 'NONE', #3552, #7716 ) ;
#8213 = CARTESIAN_POINT ( 'NONE',  ( 19.39806930854668110, 4.349999998907525089, -19.39806930854668110 ) ) ;
#8214 = CARTESIAN_POINT ( 'NONE',  ( 1.679787559701184688E-15, 0.5499999989075251561, -27.43301270000000258 ) ) ;
#8215 = CIRCLE ( 'NONE', #711, 0.4999999999999968914 ) ;
#8216 = CARTESIAN_POINT ( 'NONE',  ( 4.996790860652426159E-15, -1.462499999999999911, -2.500000000000000000 ) ) ;
#8217 = CARTESIAN_POINT ( 'NONE',  ( 0.000000000000000000, 100.0000000000000000, 0.000000000000000000 ) ) ;
#8218 = CARTESIAN_POINT ( 'NONE',  ( 27.00000000000000355, 2.249999997815050001, -11.18376618407356915 ) ) ;
#8219 = ORIENTED_EDGE ( 'NONE', *, *, #1615, .T. ) ;
#8220 = CARTESIAN_POINT ( 'NONE',  ( -21.99154324187120579, 99.50000000000001421, -9.362771248264911250 ) ) ;
#8221 = CARTESIAN_POINT ( 'NONE',  ( 3.824506687597884369, 100.0000000000000284, -24.68145443631992109 ) ) ;
#8222 = CARTESIAN_POINT ( 'NONE',  ( -15.76955986605724647, 99.49999999999998579, 15.18352214517458698 ) ) ;
#8223 = ADVANCED_FACE ( 'NONE', ( #9713 ), #192, .T. ) ;
#8224 = CARTESIAN_POINT ( 'NONE',  ( 3.739209042966563867, 100.0000000000000000, -21.42288334414699236 ) ) ;
#8225 = CARTESIAN_POINT ( 'NONE',  ( -16.63177974700816009, 100.0000000000000000, 16.59747536361813403 ) ) ;
#8226 = CARTESIAN_POINT ( 'NONE',  ( 9.468852706215191262, 99.99999999999994316, 21.22967007823213237 ) ) ;
#8227 = EDGE_LOOP ( 'NONE', ( #1125, #9020 ) ) ;
#8228 = CARTESIAN_POINT ( 'NONE',  ( -21.91899880027261460, 100.0000000000000000, -9.705014769524845875 ) ) ;
#8229 = ORIENTED_EDGE ( 'NONE', *, *, #5805, .T. ) ;
#8230 = AXIS2_PLACEMENT_3D ( 'NONE', #8159, #2519, #3204 ) ;
#8231 = CARTESIAN_POINT ( 'NONE',  ( -2.500000000000000000, -5.367390388364559506, -0.9099190197072017927 ) ) ;
#8232 = ORIENTED_EDGE ( 'NONE', *, *, #9397, .F. ) ;
#8233 = ORIENTED_EDGE ( 'NONE', *, *, #9332, .F. ) ;
#8234 = CARTESIAN_POINT ( 'NONE',  ( -22.34867803760930727, 99.99999999999995737, -10.48295844864103721 ) ) ;
#8235 = CARTESIAN_POINT ( 'NONE',  ( 3.673732336774000018, 99.99999999999997158, -21.43557726391590279 ) ) ;
#8236 = CARTESIAN_POINT ( 'NONE',  ( 4.122675185292913547, 99.49999999999997158, -22.83451320417363561 ) ) ;
#8237 = CARTESIAN_POINT ( 'NONE',  ( -15.18657300206754179, 100.0000000000000000, 16.26161032743331347 ) ) ;
#8238 = CARTESIAN_POINT ( 'NONE',  ( 8.515772100368442565, 99.50000000000000000, 20.00046577258137503 ) ) ;
#8239 = PRODUCT_RELATED_PRODUCT_CATEGORY ( 'part', '', ( #5693 ) ) ;
#8240 = B_SPLINE_CURVE_WITH_KNOTS ( 'NONE', 3,
 ( #6471, #9610, #8041, #4696, #6516, #87, #8677 ),
 .UNSPECIFIED., .F., .F.,
 ( 4, 1, 1, 1, 4 ),
 ( 0.000000000000000000, 0.2676680225848128147, 0.5230972062070123885, 0.7658030722156558001, 1.000000000000000000 ),
 .UNSPECIFIED. ) ;
#8241 = FACE_OUTER_BOUND ( 'NONE', #2086, .T. ) ;
#8242 = EDGE_CURVE ( 'NONE', #2028, #9475, #4995, .T. ) ;
#8243 = CARTESIAN_POINT ( 'NONE',  ( -21.33175168474226879, 100.0000000000000142, -11.03889704119913162 ) ) ;
#8244 = CARTESIAN_POINT ( 'NONE',  ( 9.389534246205572643, 100.0000000000000142, 21.46805835725047729 ) ) ;
#8245 = ORIENTED_EDGE ( 'NONE', *, *, #6650, .F. ) ;
#8246 = EDGE_CURVE ( 'NONE', #7350, #6241, #5426, .T. ) ;
#8247 = DIRECTION ( 'NONE',  ( -0.000000000000000000, 1.000000000000000000, -0.000000000000000000 ) ) ;
#8248 = CARTESIAN_POINT ( 'NONE',  ( -19.39806930854667755, 2.249999998907525001, -19.39806930854668110 ) ) ;
#8249 = CARTESIAN_POINT ( 'NONE',  ( -15.32348647777738826, 99.50000000000000000, 15.39505148541300450 ) ) ;
#8250 = DIRECTION ( 'NONE',  ( 0.000000000000000000, 0.000000000000000000, -1.000000000000000000 ) ) ;
#8251 = CARTESIAN_POINT ( 'NONE',  ( 7.826802610544922878, 99.50000000000000000, 21.21129867192371421 ) ) ;
#8252 = EDGE_CURVE ( 'NONE', #3336, #1163, #920, .T. ) ;
#8253 = CARTESIAN_POINT ( 'NONE',  ( 3.306546357697854128E-15, 100.0000000000000000, 27.00000000000000355 ) ) ;
#8254 = CARTESIAN_POINT ( 'NONE',  ( -27.00000000000000355, 4.199999997815050179, -3.306546357697854128E-15 ) ) ;
#8255 = CARTESIAN_POINT ( 'NONE',  ( -20.69312081029678296, 99.49999999999997158, -9.926742041671966277 ) ) ;
#8256 = CARTESIAN_POINT ( 'NONE',  ( -21.04016555629948826, 99.50000000000001421, -9.929603401003973318 ) ) ;
#8257 = PLANE ( 'NONE',  #1720 ) ;
#8258 = CARTESIAN_POINT ( 'NONE',  ( -21.58460863908062066, 100.0000000000000284, -11.10356610083683648 ) ) ;
#8259 = DIRECTION ( 'NONE',  ( -0.9985036676371303876, 0.000000000000000000, 0.05468478504300072762 ) ) ;
#8260 = CARTESIAN_POINT ( 'NONE',  ( -2.500000000000000000, -4.931249998770965703, -1.443375672974064106 ) ) ;
#8261 = EDGE_CURVE ( 'NONE', #7095, #3170, #1898, .T. ) ;
#8262 = CARTESIAN_POINT ( 'NONE',  ( 1.128215178124999607, -4.790624999385483029, -1.954126010382871259 ) ) ;
#8263 =( NAMED_UNIT ( * ) SI_UNIT ( $, .STERADIAN. ) SOLID_ANGLE_UNIT ( ) );
#8264 = CARTESIAN_POINT ( 'NONE',  ( -15.07178375341841381, 99.50000000000000000, 16.66969090848992607 ) ) ;
#8265 = EDGE_CURVE ( 'NONE', #7818, #2647, #1847, .T. ) ;
#8266 = DIRECTION ( 'NONE',  ( -0.000000000000000000, 1.000000000000000000, -0.000000000000000000 ) ) ;
#8267 = CARTESIAN_POINT ( 'NONE',  ( -27.43301270000000969, 3.899999998907524912, 11.36312591709335429 ) ) ;
#8268 = CARTESIAN_POINT ( 'NONE',  ( 1.653273178848927064E-15, 0.2000000000000000111, -27.00000000000000355 ) ) ;
#8269 = CARTESIAN_POINT ( 'NONE',  ( -19.75840245672548789, 99.50000000000000000, -8.735905494466331689 ) ) ;
#8270 = FACE_OUTER_BOUND ( 'NONE', #7661, .T. ) ;
#8271 = CIRCLE ( 'NONE', #5927, 1.324999999999999956 ) ;
#8272 = ORIENTED_EDGE ( 'NONE', *, *, #8840, .F. ) ;
#8273 = CARTESIAN_POINT ( 'NONE',  ( 7.978247738654171251, 99.50000000000000000, 20.00924965157036794 ) ) ;
#8274 = CARTESIAN_POINT ( 'NONE',  ( -19.39806930854668465, 4.749999998907525445, 19.39806930854667755 ) ) ;
#8275 = DIRECTION ( 'NONE',  ( -0.000000000000000000, 1.000000000000000000, -0.000000000000000000 ) ) ;
#8276 = CARTESIAN_POINT ( 'NONE',  ( -2.256430356250000102, -5.203124999385482674, 0.000000000000000000 ) ) ;
#8277 = CARTESIAN_POINT ( 'NONE',  ( 9.877377282685029372E-16, -4.387499999999999289, 2.500000000000000000 ) ) ;
#8278 = AXIS2_PLACEMENT_3D ( 'NONE', #8046, #5644, #7155 ) ;
#8279 = CARTESIAN_POINT ( 'NONE',  ( 0.000000000000000000, 0.000000000000000000, 0.000000000000000000 ) ) ;
#8280 = CARTESIAN_POINT ( 'NONE',  ( -21.38163724633288965, 100.0000000000000568, -9.681902434707239991 ) ) ;
#8281 = DIRECTION ( 'NONE',  ( -0.9197984731044490658, 0.000000000000000000, 0.3923910917372159246 ) ) ;
#8282 = CARTESIAN_POINT ( 'NONE',  ( -1.249999999999998224, -3.468749998770965348, 2.165063509461097713 ) ) ;
#8283 = ORIENTED_EDGE ( 'NONE', *, *, #10227, .T. ) ;
#8284 = CARTESIAN_POINT ( 'NONE',  ( -22.34945848979098670, 100.0000000000000000, -10.27225542379191481 ) ) ;
#8285 = CARTESIAN_POINT ( 'NONE',  ( 3.214822648120007731, 99.99999999999997158, -21.86319392453323829 ) ) ;
#8286 = CARTESIAN_POINT ( 'NONE',  ( -3.000000000000000888, -15.00000000000000000, -1.732050807568877415 ) ) ;
#8287 = CARTESIAN_POINT ( 'NONE',  ( 3.061616997868383141E-16, 0.000000000000000000, 2.500000000000000000 ) ) ;
#8288 = EDGE_CURVE ( 'NONE', #9210, #2107, #5041, .T. ) ;
#8289 = DIRECTION ( 'NONE',  ( -0.000000000000000000, 1.000000000000000000, -0.000000000000000000 ) ) ;
#8290 = VECTOR ( 'NONE', #10050, 1000.000000000000000 ) ;
#8291 = CARTESIAN_POINT ( 'NONE',  ( 21.43339342948717885, 99.50000000000000000, -1.392427884615384803 ) ) ;
#8292 = DIRECTION ( 'NONE',  ( 0.000000000000000000, 1.000000000000000000, 0.000000000000000000 ) ) ;
#8293 = CARTESIAN_POINT ( 'NONE',  ( 9.838488147574068421, 100.0000000000000000, 20.25735696016189280 ) ) ;
#8294 = ORIENTED_EDGE ( 'NONE', *, *, #4984, .T. ) ;
#8295 = AXIS2_PLACEMENT_3D ( 'NONE', #3880, #7068, #4819 ) ;
#8296 = DIRECTION ( 'NONE',  ( -0.000000000000000000, 1.000000000000000000, -0.000000000000000000 ) ) ;
#8297 = CARTESIAN_POINT ( 'NONE',  ( -27.43301270000000969, 4.799999998907525267, 11.36312591709335429 ) ) ;
#8298 = CARTESIAN_POINT ( 'NONE',  ( -23.82500000000000284, 72.50000000000001421, 0.000000000000000000 ) ) ;
#8299 = CARTESIAN_POINT ( 'NONE',  ( -0.6698729810778020211, -4.592403810567665445, -2.500000000000002665 ) ) ;
#8300 = CARTESIAN_POINT ( 'NONE',  ( 7.783718120363267268, 99.99999999999994316, 21.09473326129887027 ) ) ;
#8301 = CARTESIAN_POINT ( 'NONE',  ( 3.341734429721257005, 100.0000000000000284, -22.34498040423979148 ) ) ;
#8302 = CARTESIAN_POINT ( 'NONE',  ( 26.99999999999999645, 2.949999997815051067, 11.18376618407358691 ) ) ;
#8303 = FACE_OUTER_BOUND ( 'NONE', #10250, .T. ) ;
#8304 = CARTESIAN_POINT ( 'NONE',  ( 2.500000000000000000, -4.631249998770966769, -1.443375672974065438 ) ) ;
#8305 = LINE ( 'NONE', #5210, #211 ) ;
#8306 = CARTESIAN_POINT ( 'NONE',  ( 4.185097728209222545, 99.50000000000000000, -21.50746221358744847 ) ) ;
#8307 = CARTESIAN_POINT ( 'NONE',  ( 0.000000000000000000, 75.00000000000001421, 23.99999999999999645 ) ) ;
#8308 = PRODUCT_DEFINITION_FORMATION_WITH_SPECIFIED_SOURCE ( 'ANY', '', #1333, .NOT_KNOWN. ) ;
#8309 = CARTESIAN_POINT ( 'NONE',  ( -1.249999999999998224, -4.818749998770964993, 2.165063509461097713 ) ) ;
#8310 = ORIENTED_EDGE ( 'NONE', *, *, #8691, .T. ) ;
#8311 = CARTESIAN_POINT ( 'NONE',  ( -2.500000000000000000, -1.349999999999999867, 0.000000000000000000 ) ) ;
#8312 = FILL_AREA_STYLE_COLOUR ( '', #284 ) ;
#8313 = CARTESIAN_POINT ( 'NONE',  ( -15.29853103387017121, 99.50000000000001421, 14.98378122532347057 ) ) ;
#8314 = DIRECTION ( 'NONE',  ( -0.000000000000000000, -0.000000000000000000, 1.000000000000000000 ) ) ;
#8315 = EDGE_CURVE ( 'NONE', #1699, #9838, #3480, .T. ) ;
#8316 = CARTESIAN_POINT ( 'NONE',  ( -19.39806930854667755, 2.949999998907525178, -19.39806930854668110 ) ) ;
#8317 = CARTESIAN_POINT ( 'NONE',  ( -27.43301270000000258, 0.6999999989075252893, -11.36312591709336317 ) ) ;
#8318 = ADVANCED_FACE ( 'NONE', ( #1123 ), #6665, .T. ) ;
#8319 = DIRECTION ( 'NONE',  ( 0.000000000000000000, 0.000000000000000000, 1.000000000000000000 ) ) ;
#8320 = VECTOR ( 'NONE', #9928, 1000.000000000000000 ) ;
#8321 = DIRECTION ( 'NONE',  ( -0.000000000000000000, -1.000000000000000000, -0.000000000000000000 ) ) ;
#8322 = DIRECTION ( 'NONE',  ( 0.000000000000000000, -1.000000000000000000, 0.000000000000000000 ) ) ;
#8323 = B_SPLINE_CURVE_WITH_KNOTS ( 'NONE', 3,
 ( #7536, #8228, #1060, #5976, #4252, #6655, #7487, #326, #9168, #8280, #5187, #1109, #9846, #1884, #2681, #8385, #9897, #5920, #8661 ),
 .UNSPECIFIED., .F., .F.,
 ( 4, 1, 1, 1, 1, 1, 1, 1, 1, 1, 1, 1, 1, 1, 1, 1, 4 ),
 ( 0.000000000000000000, 0.06505403082392276215, 0.1283503816230405770, 0.1902281050068566903, 0.2509397092642763338, 0.3119571365542418429, 0.3738829716944830350, 0.4367040802691206092, 0.5009896104483916313, 0.5655726868558689224, 0.6286067690057803858, 0.6898677555008378981, 0.7506620835893632604, 0.8110632348575060879, 0.8726242918051292374, 0.9355756365154705989, 0.9999999999999998890 ),
 .UNSPECIFIED. ) ;
#8324 = VERTEX_POINT ( 'NONE', #3586 ) ;
#8325 = PLANE ( 'NONE',  #5120 ) ;
#8326 = CARTESIAN_POINT ( 'NONE',  ( -0.6698729810778105698, -5.251346188203299903, 2.499999999999997780 ) ) ;
#8327 = CARTESIAN_POINT ( 'NONE',  ( 1.128215178125001161, -0.4406249993854829405, 1.954126010382870815 ) ) ;
#8328 = CARTESIAN_POINT ( 'NONE',  ( -15.98972951825121669, 99.49999999999997158, 15.19400804711857411 ) ) ;
#8329 = VECTOR ( 'NONE', #1173, 1000.000000000000000 ) ;
#8330 = CARTESIAN_POINT ( 'NONE',  ( 0.000000000000000000, 0.000000000000000000, 0.000000000000000000 ) ) ;
#8331 = LINE ( 'NONE', #273, #5450 ) ;
#8332 = DIRECTION ( 'NONE',  ( 0.000000000000000000, 0.000000000000000000, -1.000000000000000000 ) ) ;
#8333 = ORIENTED_EDGE ( 'NONE', *, *, #9948, .T. ) ;
#8334 = DIRECTION ( 'NONE',  ( 0.000000000000000000, 1.000000000000000000, 0.000000000000000000 ) ) ;
#8335 = CARTESIAN_POINT ( 'NONE',  ( 2.256430356249999658, -1.790624999385482807, -1.302750673588581432 ) ) ;
#8336 = VERTEX_POINT ( 'NONE', #7664 ) ;
#8337 = CARTESIAN_POINT ( 'NONE',  ( -22.31427554260534052, 100.0000000000000000, -10.13077409178744404 ) ) ;
#8338 = LINE ( 'NONE', #1168, #1616 ) ;
#8339 = VECTOR ( 'NONE', #8289, 1000.000000000000000 ) ;
#8340 = CARTESIAN_POINT ( 'NONE',  ( -4.959819536546781389E-15, 5.199999997815050179, 27.00000000000000355 ) ) ;
#8341 = CARTESIAN_POINT ( 'NONE',  ( -15.13520964245927836, 99.99999999999998579, 15.69931698147095034 ) ) ;
#8342 = CARTESIAN_POINT ( 'NONE',  ( -4.959819536546781389E-15, 3.000000000000000000, 27.00000000000000355 ) ) ;
#8343 = CARTESIAN_POINT ( 'NONE',  ( 3.306546357697854128E-15, 100.0000000000000000, 27.00000000000000355 ) ) ;
#8344 = CARTESIAN_POINT ( 'NONE',  ( 1.034219503716432668E-14, -3.656249998770965792, -2.500000000000000000 ) ) ;
#8345 = CARTESIAN_POINT ( 'NONE',  ( 9.500395184910136237, 100.0000000000000000, 21.12540332933289733 ) ) ;
#8346 = EDGE_LOOP ( 'NONE', ( #4203, #2096, #9372, #8405, #6481, #9312, #1100, #7537, #2738, #1359, #4012, #1190, #8080, #557, #9887, #5996 ) ) ;
#8347 = DIRECTION ( 'NONE',  ( 0.000000000000000000, 1.000000000000000000, 0.000000000000000000 ) ) ;
#8348 = CARTESIAN_POINT ( 'NONE',  ( 1.679787559701184688E-15, 4.549999998907526155, -27.43301270000000258 ) ) ;
#8349 = DIRECTION ( 'NONE',  ( 0.000000000000000000, 1.000000000000000000, 0.000000000000000000 ) ) ;
#8350 = EDGE_CURVE ( 'NONE', #2028, #10197, #5912, .T. ) ;
#8351 = CARTESIAN_POINT ( 'NONE',  ( 4.135809822336132591, 99.49999999999998579, -24.70305975188825443 ) ) ;
#8352 = CARTESIAN_POINT ( 'NONE',  ( 19.09188309203678102, 4.499999997815050001, 19.09188309203678813 ) ) ;
#8353 = EDGE_LOOP ( 'NONE', ( #230, #3907, #8613 ) ) ;
#8354 = CARTESIAN_POINT ( 'NONE',  ( 9.915951879163557692, 99.50000000000002842, 20.63215000232408158 ) ) ;
#8355 = CARTESIAN_POINT ( 'NONE',  ( -4.959819536546781389E-15, 3.599999997815050534, 27.00000000000000355 ) ) ;
#8356 = CARTESIAN_POINT ( 'NONE',  ( 11.18376618407357093, 3.350000000000000089, -27.00000000000000355 ) ) ;
#8357 = DIRECTION ( 'NONE',  ( -0.000000000000000000, 1.000000000000000000, -0.000000000000000000 ) ) ;
#8358 = CARTESIAN_POINT ( 'NONE',  ( 3.817429849879703241, 99.99999999999998579, -22.92346308580664171 ) ) ;
#8359 = ORIENTED_EDGE ( 'NONE', *, *, #1008, .F. ) ;
#8360 = DIRECTION ( 'NONE',  ( 0.000000000000000000, -1.000000000000000000, 0.000000000000000000 ) ) ;
#8361 = CARTESIAN_POINT ( 'NONE',  ( -2.500000000000000000, -4.893749998770965171, 0.000000000000000000 ) ) ;
#8362 = ORIENTED_EDGE ( 'NONE', *, *, #5641, .F. ) ;
#8363 = MECHANICAL_DESIGN_GEOMETRIC_PRESENTATION_REPRESENTATION (  '', ( #510 ), #8877 ) ;
#8364 = CARTESIAN_POINT ( 'NONE',  ( -1.250000000000000222, -1.424999999999999822, -2.165063509461096825 ) ) ;
#8365 = ADVANCED_FACE ( 'NONE', ( #2971 ), #7454, .T. ) ;
#8366 = SHAPE_DEFINITION_REPRESENTATION ( #1, #5114 ) ;
#8367 = CARTESIAN_POINT ( 'NONE',  ( -14.78677372028383097, 99.49999999999998579, 15.63810349997947569 ) ) ;
#8368 = CARTESIAN_POINT ( 'NONE',  ( 2.256430356250000102, -0.4781249993854829183, -2.763330213280484622E-16 ) ) ;
#8369 = CARTESIAN_POINT ( 'NONE',  ( -5.039362679103552881E-15, 2.449999998907525178, 27.43301270000000258 ) ) ;
#8370 = CARTESIAN_POINT ( 'NONE',  ( -20.45905772418405988, 100.0000000000000000, -10.59533404166311321 ) ) ;
#8371 = CARTESIAN_POINT ( 'NONE',  ( -15.98658610793439117, 100.0000000000000142, 14.83943845084690949 ) ) ;
#8372 = PLANE ( 'NONE',  #4306 ) ;
#8373 = CARTESIAN_POINT ( 'NONE',  ( 3.970307086022987431, 100.0000000000000142, -24.36314111580913178 ) ) ;
#8374 = ORIENTED_EDGE ( 'NONE', *, *, #5282, .T. ) ;
#8375 = CARTESIAN_POINT ( 'NONE',  ( 7.826802610544922878, 99.50000000000000000, 21.21129867192371421 ) ) ;
#8376 = CARTESIAN_POINT ( 'NONE',  ( 2.912748042341355870, 99.99999999999998579, -22.34826719014139940 ) ) ;
#8377 = ORIENTED_EDGE ( 'NONE', *, *, #6915, .T. ) ;
#8378 = ADVANCED_FACE ( 'NONE', ( #4524 ), #6094, .T. ) ;
#8379 = CARTESIAN_POINT ( 'NONE',  ( 2.256430356249999658, -0.7781249993854829627, -1.302750673588581432 ) ) ;
#8380 = CARTESIAN_POINT ( 'NONE',  ( -27.43301270000000258, 0.5999999989075250895, -11.36312591709336317 ) ) ;
#8381 = ADVANCED_FACE ( 'NONE', ( #391 ), #3807, .T. ) ;
#8382 = CARTESIAN_POINT ( 'NONE',  ( 26.99999999999999645, 4.750000000000000000, 11.18376618407358691 ) ) ;
#8383 = AXIS2_PLACEMENT_3D ( 'NONE', #1451, #718, #3913 ) ;
#8384 = CARTESIAN_POINT ( 'NONE',  ( 9.513000527211589841, 99.99999999999994316, 20.35102222961602436 ) ) ;
#8385 = CARTESIAN_POINT ( 'NONE',  ( -21.04016555629948826, 100.0000000000000142, -9.929603401003973318 ) ) ;
#8386 = EDGE_LOOP ( 'NONE', ( #6744, #8933 ) ) ;
#8387 = CARTESIAN_POINT ( 'NONE',  ( -15.83671465916681242, 100.0000000000000000, 16.65403364262263608 ) ) ;
#8388 = CARTESIAN_POINT ( 'NONE',  ( 2.256430356250000546, -1.865624999385482985, 1.302750673588579877 ) ) ;
#8389 = ORIENTED_EDGE ( 'NONE', *, *, #6951, .F. ) ;
#8390 = VECTOR ( 'NONE', #8519, 1000.000000000000000 ) ;
#8391 = CARTESIAN_POINT ( 'NONE',  ( 4.693123912524271191, 99.50000000000002842, -24.12247278045041554 ) ) ;
#8392 = CARTESIAN_POINT ( 'NONE',  ( 27.43301269999999548, 0.9999999989075253337, 11.36312591709337916 ) ) ;
#8393 = CARTESIAN_POINT ( 'NONE',  ( -4.959819536546781389E-15, 0.6000000000000000888, 27.00000000000000355 ) ) ;
#8394 = CARTESIAN_POINT ( 'NONE',  ( -15.31787750341841559, 100.0000000000000000, 16.43551622900274722 ) ) ;
#8395 = DIRECTION ( 'NONE',  ( 0.000000000000000000, 0.000000000000000000, -1.000000000000000000 ) ) ;
#8396 = CARTESIAN_POINT ( 'NONE',  ( -16.67860655220511035, 99.99999999999998579, 15.23428378554110374 ) ) ;
#8397 = CARTESIAN_POINT ( 'NONE',  ( -15.09818093130665773, 99.50000000000000000, 16.69478731934044191 ) ) ;
#8398 = VECTOR ( 'NONE', #6439, 1000.000000000000227 ) ;
#8399 = ORIENTED_EDGE ( 'NONE', *, *, #2242, .T. ) ;
#8400 = DIRECTION ( 'NONE',  ( 0.9766186814179788067, 0.000000000000000000, -0.2149789550291109352 ) ) ;
#8401 = PRESENTATION_LAYER_ASSIGNMENT (  '', '', ( #2563 ) ) ;
#8402 = CARTESIAN_POINT ( 'NONE',  ( -5.039362679103552881E-15, 4.149999998907524912, 27.43301270000000258 ) ) ;
#8403 = DIRECTION ( 'NONE',  ( -0.08704561088320925122, 0.9949358851208914833, 0.05025580687519626277 ) ) ;
#8404 = DIRECTION ( 'NONE',  ( 0.8660254037844385966, -0.000000000000000000, -0.5000000000000000000 ) ) ;
#8405 = ORIENTED_EDGE ( 'NONE', *, *, #967, .F. ) ;
#8406 = CARTESIAN_POINT ( 'NONE',  ( -23.82500000000000284, 0.000000000000000000, 0.000000000000000000 ) ) ;
#8407 = CARTESIAN_POINT ( 'NONE',  ( 5.179363668139080445, 99.50000000000007105, -23.94265746362379943 ) ) ;
#8408 = CARTESIAN_POINT ( 'NONE',  ( -2.500000000000000000, -3.993749998770965703, 0.000000000000000000 ) ) ;
#8409 = DIRECTION ( 'NONE',  ( 0.000000000000000000, 0.000000000000000000, -1.000000000000000000 ) ) ;
#8410 = DIRECTION ( 'NONE',  ( 0.000000000000000000, 1.000000000000000000, 0.000000000000000000 ) ) ;
#8411 = EDGE_CURVE ( 'NONE', #7177, #9070, #9017, .T. ) ;
#8412 = EDGE_LOOP ( 'NONE', ( #7019, #1297, #10007, #3781 ) ) ;
#8413 = CARTESIAN_POINT ( 'NONE',  ( -16.12578516900833137, 99.50000000000001421, 15.23469143358620492 ) ) ;
#8414 = CARTESIAN_POINT ( 'NONE',  ( 11.36312591709336139, 2.099999998907525089, -27.43301270000000258 ) ) ;
#8415 = ORIENTED_EDGE ( 'NONE', *, *, #531, .T. ) ;
#8416 = CARTESIAN_POINT ( 'NONE',  ( 1.249999999999999334, -2.399999999999999911, -2.165063509461096825 ) ) ;
#8417 = APPLICATION_PROTOCOL_DEFINITION ( 'draft international standard', 'automotive_design', 1998, #5122 ) ;
#8418 = FACE_OUTER_BOUND ( 'NONE', #10106, .T. ) ;
#8419 = CARTESIAN_POINT ( 'NONE',  ( 2.256430356250000102, -2.728124999385482585, -2.763330213280484622E-16 ) ) ;
#8420 = CARTESIAN_POINT ( 'NONE',  ( -5.039362679103552881E-15, 1.649999998907525356, 27.43301270000000258 ) ) ;
#8421 = CARTESIAN_POINT ( 'NONE',  ( 7.156925775808251622, 99.50000000000000000, 23.91622092442889524 ) ) ;
#8422 = EDGE_LOOP ( 'NONE', ( #5747, #2822, #648, #2019 ) ) ;
#8423 = CARTESIAN_POINT ( 'NONE',  ( -15.07178375341841559, 100.0000000000000142, 15.16157792772069968 ) ) ;
#8424 = DIRECTION ( 'NONE',  ( 0.000000000000000000, -1.000000000000000000, 0.000000000000000000 ) ) ;
#8425 = SURFACE_STYLE_USAGE ( .BOTH. , #6747 ) ;
#8426 = EDGE_CURVE ( 'NONE', #2804, #1454, #6586, .T. ) ;
#8427 = EDGE_CURVE ( 'NONE', #5650, #6302, #2014, .T. ) ;
#8428 = CARTESIAN_POINT ( 'NONE',  ( 4.232798786556307036, 100.0000000000000000, -24.34936571594186105 ) ) ;
#8429 = CARTESIAN_POINT ( 'NONE',  ( -1.128215178124998497, -1.865624999385482763, 1.954126010382872147 ) ) ;
#8430 = CARTESIAN_POINT ( 'NONE',  ( -2.256430356250000102, -0.2531249993854829405, 0.000000000000000000 ) ) ;
#8431 = ORIENTED_EDGE ( 'NONE', *, *, #237, .T. ) ;
#8432 = CARTESIAN_POINT ( 'NONE',  ( 4.786228327491941173E-16, -0.9281249993854827629, 2.605501347177161087 ) ) ;
#8433 = CARTESIAN_POINT ( 'NONE',  ( 19.39806930854668110, 1.949999998907525178, -19.39806930854668110 ) ) ;
#8434 = ORIENTED_EDGE ( 'NONE', *, *, #1792, .F. ) ;
#8435 = CARTESIAN_POINT ( 'NONE',  ( -7.500000000000000888, 105.0000000000000142, 3.000000000000000000 ) ) ;
#8436 = CARTESIAN_POINT ( 'NONE',  ( 7.156925775808251622, 99.50000000000000000, 23.91622092442889524 ) ) ;
#8437 = CARTESIAN_POINT ( 'NONE',  ( 1.653273178848927064E-15, 2.600000000000000533, -27.00000000000000355 ) ) ;
#8438 = ORIENTED_EDGE ( 'NONE', *, *, #1823, .T. ) ;
#8439 = VECTOR ( 'NONE', #1081, 1000.000000000000000 ) ;
#8440 = CARTESIAN_POINT ( 'NONE',  ( 4.803433990161294354, 100.0000000000000142, -23.96838578116891583 ) ) ;
#8441 = CARTESIAN_POINT ( 'NONE',  ( -1.128215178125000273, -2.578124999385482674, -1.954126010382871259 ) ) ;
#8442 = ORIENTED_EDGE ( 'NONE', *, *, #6647, .F. ) ;
#8443 = CARTESIAN_POINT ( 'NONE',  ( -22.21584973381871464, 99.50000000000001421, -9.938501092090024969 ) ) ;
#8444 = DIRECTION ( 'NONE',  ( -0.000000000000000000, -1.000000000000000000, 0.000000000000000000 ) ) ;
#8445 = CARTESIAN_POINT ( 'NONE',  ( -21.31369174262763622, 99.49999999999997158, -9.710155485040722567 ) ) ;
#8446 = AXIS2_PLACEMENT_3D ( 'NONE', #4957, #1911, #1134 ) ;
#8447 = CARTESIAN_POINT ( 'NONE',  ( 1.034219503716432668E-14, -5.006249998770964993, -2.500000000000000000 ) ) ;
#8448 = CARTESIAN_POINT ( 'NONE',  ( 3.302864939465488536, 100.0000000000000142, -22.83905924565489443 ) ) ;
#8449 = ORIENTED_EDGE ( 'NONE', *, *, #8746, .T. ) ;
#8450 = EDGE_CURVE ( 'NONE', #8484, #3366, #7552, .T. ) ;
#8451 = CARTESIAN_POINT ( 'NONE',  ( 3.306546357697854128E-15, 100.0000000000000000, 27.00000000000000355 ) ) ;
#8452 = CARTESIAN_POINT ( 'NONE',  ( -11.18376618407356737, 1.050000000000000044, -27.00000000000000355 ) ) ;
#8453 = CARTESIAN_POINT ( 'NONE',  ( 9.513000527211589841, 100.0000000000000000, 20.35102222961602436 ) ) ;
#8454 =( BOUNDED_CURVE ( )  B_SPLINE_CURVE ( 2, ( #6557, #818, #2540, #9748, #4789, #7244, #7986, #5733, #7196 ),
 .UNSPECIFIED., .F., .T. ) 
 B_SPLINE_CURVE_WITH_KNOTS ( ( 3, 2, 2, 2, 3 ),
 ( 0.8214285714285713969, 0.8392857142857143016, 0.8571428571428570953, 0.8750000000000000000, 0.8928571428571429047 ),
 .UNSPECIFIED. ) 
 CURVE ( )  GEOMETRIC_REPRESENTATION_ITEM ( )  RATIONAL_B_SPLINE_CURVE ( ( 1.000000000000000000, 0.9238795325112867385, 1.000000000000000000, 0.9238795325112867385, 1.000000000000000000, 0.9238795325112867385, 1.000000000000000000, 0.9238795325112867385, 1.000000000000000000 ) ) 
 REPRESENTATION_ITEM ( '' )  );
#8455 = ORIENTED_EDGE ( 'NONE', *, *, #2793, .T. ) ;
#8456 = DIRECTION ( 'NONE',  ( 0.000000000000000000, 0.000000000000000000, -1.000000000000000000 ) ) ;
#8457 = CARTESIAN_POINT ( 'NONE',  ( -27.43301270000000258, 4.749999998907525445, -3.359575119402369376E-15 ) ) ;
#8458 = CARTESIAN_POINT ( 'NONE',  ( 2.256430356250000102, -2.615624999385482763, -2.763330213280484622E-16 ) ) ;
#8459 = DIRECTION ( 'NONE',  ( 0.9789429660840186509, 0.000000000000000000, -0.2041339490496966447 ) ) ;
#8460 = ORIENTED_EDGE ( 'NONE', *, *, #1417, .T. ) ;
#8461 = FACE_OUTER_BOUND ( 'NONE', #10194, .T. ) ;
#8462 = VECTOR ( 'NONE', #5192, 1000.000000000000000 ) ;
#8463 = DIRECTION ( 'NONE',  ( 0.000000000000000000, 0.000000000000000000, 1.000000000000000000 ) ) ;
#8464 = DIRECTION ( 'NONE',  ( 0.000000000000000000, 0.000000000000000000, -1.000000000000000000 ) ) ;
#8465 = CARTESIAN_POINT ( 'NONE',  ( -16.45391695211397831, 99.50000000000004263, 16.32580124622701589 ) ) ;
#8466 = CARTESIAN_POINT ( 'NONE',  ( -2.500000000000000000, -0.4874999999999999889, -1.443375672974064106 ) ) ;
#8467 = EDGE_LOOP ( 'NONE', ( #6908, #7208, #1983, #1226 ) ) ;
#8468 = CARTESIAN_POINT ( 'NONE',  ( -15.62751930918662069, 99.49999999999998579, 15.20915780906945436 ) ) ;
#8469 = CARTESIAN_POINT ( 'NONE',  ( 27.43301270000000258, 1.199999998907525178, -11.36312591709336139 ) ) ;
#8470 = ORIENTED_EDGE ( 'NONE', *, *, #1973, .F. ) ;
#8471 = VECTOR ( 'NONE', #10149, 1000.000000000000000 ) ;
#8472 = CARTESIAN_POINT ( 'NONE',  ( -2.500000000000000000, -0.9000000000000000222, 0.000000000000000000 ) ) ;
#8473 = APPLICATION_PROTOCOL_DEFINITION ( 'draft international standard', 'automotive_design', 1998, #2595 ) ;
#8474 = CARTESIAN_POINT ( 'NONE',  ( 8.684839681857363658, 99.50000000000001421, 19.94043386883836178 ) ) ;
#8475 = DIRECTION ( 'NONE',  ( -0.6427814120798343023, 4.154457043096084790E-06, 0.7660496434744911154 ) ) ;
#8476 = CARTESIAN_POINT ( 'NONE',  ( 2.256430356250000546, -0.9656249993854827407, 1.302750673588579877 ) ) ;
#8477 = CARTESIAN_POINT ( 'NONE',  ( 4.852629679480013891, 99.50000000000001421, -23.84752007312514621 ) ) ;
#8478 = CARTESIAN_POINT ( 'NONE',  ( -27.43301270000000969, 0.7999999989075252671, 11.36312591709335429 ) ) ;
#8479 = CARTESIAN_POINT ( 'NONE',  ( -15.37123125604856710, 100.0000000000000142, 16.48683530611566539 ) ) ;
#8480 = AXIS2_PLACEMENT_3D ( 'NONE', #7326, #3662, #2930 ) ;
#8481 = LINE ( 'NONE', #7692, #9666 ) ;
#8482 = CARTESIAN_POINT ( 'NONE',  ( 7.771508748547515388, 100.0000000000000142, 20.40818475981234315 ) ) ;
#8483 = CARTESIAN_POINT ( 'NONE',  ( -15.62751930918662069, 99.99999999999998579, 15.20915780906945436 ) ) ;
#8484 = VERTEX_POINT ( 'NONE', #7199 ) ;
#8485 = CARTESIAN_POINT ( 'NONE',  ( 2.256430356250000546, -2.203124999385482674, 1.302750673588579877 ) ) ;
#8486 = CARTESIAN_POINT ( 'NONE',  ( 1.034219503716432668E-14, -4.162500000000000533, -2.500000000000000000 ) ) ;
#8487 = ORIENTED_EDGE ( 'NONE', *, *, #5432, .T. ) ;
#8488 = CARTESIAN_POINT ( 'NONE',  ( 27.00000000000000355, 0.5999999978150503122, 0.000000000000000000 ) ) ;
#8489 = CARTESIAN_POINT ( 'NONE',  ( -27.43301270000000258, 2.999999998907525445, -11.36312591709336317 ) ) ;
#8490 =( LENGTH_UNIT ( ) NAMED_UNIT ( * ) SI_UNIT ( .MILLI., .METRE. ) );
#8491 = VERTEX_POINT ( 'NONE', #86 ) ;
#8492 = EDGE_CURVE ( 'NONE', #7765, #4647, #8729, .T. ) ;
#8493 = CARTESIAN_POINT ( 'NONE',  ( 11.18376618407357626, 1.450000000000000400, 27.00000000000000000 ) ) ;
#8494 = CIRCLE ( 'NONE', #144, 30.00000000000000000 ) ;
#8495 = LINE ( 'NONE', #1431, #1604 ) ;
#8496 = ORIENTED_EDGE ( 'NONE', *, *, #4844, .F. ) ;
#8497 = DIRECTION ( 'NONE',  ( 0.4980973490458731057, -0.08715574274765838791, -0.8627299156628207566 ) ) ;
#8498 = CARTESIAN_POINT ( 'NONE',  ( -1.128215178124998497, -2.878124999385482496, 1.954126010382872147 ) ) ;
#8499 = ORIENTED_EDGE ( 'NONE', *, *, #7813, .F. ) ;
#8500 = AXIS2_PLACEMENT_3D ( 'NONE', #1815, #6679, #5109 ) ;
#8501 = LINE ( 'NONE', #10011, #614 ) ;
#8502 = CARTESIAN_POINT ( 'NONE',  ( 27.43301270000000258, 0.2999999989075252671, -11.36312591709336139 ) ) ;
#8503 = DIRECTION ( 'NONE',  ( 0.000000000000000000, -1.000000000000000000, 0.000000000000000000 ) ) ;
#8504 = CARTESIAN_POINT ( 'NONE',  ( 1.128215178125001161, -1.453124999385482896, 1.954126010382870815 ) ) ;
#8505 = CARTESIAN_POINT ( 'NONE',  ( 5.242860087038358152, 99.50000000000002842, -23.52699316036146371 ) ) ;
#8506 = CARTESIAN_POINT ( 'NONE',  ( 4.820889542125314620, 99.49999999999998579, -21.76289454767624676 ) ) ;
#8507 = DIRECTION ( 'NONE',  ( -0.000000000000000000, -0.000000000000000000, -1.000000000000000000 ) ) ;
#8508 = CARTESIAN_POINT ( 'NONE',  ( 1.250000000000001110, -2.999999999999999556, 2.165063509461096380 ) ) ;
#8509 = EDGE_LOOP ( 'NONE', ( #4823, #6196 ) ) ;
#8510 = EDGE_CURVE ( 'NONE', #4631, #2830, #6645, .T. ) ;
#8511 = CARTESIAN_POINT ( 'NONE',  ( -22.10910773081910818, 99.50000000000001421, -11.33820747227609793 ) ) ;
#8512 = CARTESIAN_POINT ( 'NONE',  ( 0.6698729810778112359, -4.182596189432334022, -2.499999999999996447 ) ) ;
#8513 = CARTESIAN_POINT ( 'NONE',  ( -1.128215178125000273, -2.015624999385483118, -1.954126010382871259 ) ) ;
#8514 = ADVANCED_FACE ( 'NONE', ( #823 ), #583, .T. ) ;
#8515 = CARTESIAN_POINT ( 'NONE',  ( 9.897596448871711416, 99.99999999999997158, 20.85734708541456328 ) ) ;
#8516 = B_SPLINE_SURFACE_WITH_KNOTS ( 'NONE', 3, 1, ( 
 ( #150, #2557 ),
 ( #4028, #8153 ),
 ( #195, #2455 ),
 ( #6431, #3378 ),
 ( #9761, #8197 ),
 ( #1668, #7400 ),
 ( #242, #2648 ) ),
 .UNSPECIFIED., .F., .F., .F.,
 ( 4, 1, 1, 1, 4 ),
 ( 2, 2 ),
 ( 0.000000000000000000, 0.2581490702850675056, 0.5078756004687992043, 0.7540928115589713432, 1.000000000000000000 ),
 ( 0.000000000000000000, 1.000000000000000000 ),
 .UNSPECIFIED. ) ;
#8517 = VERTEX_POINT ( 'NONE', #10352 ) ;
#8518 = CARTESIAN_POINT ( 'NONE',  ( 0.000000000000000000, 5.000000000000000000, 0.000000000000000000 ) ) ;
#8519 = DIRECTION ( 'NONE',  ( -0.000000000000000000, 1.000000000000000000, -0.000000000000000000 ) ) ;
#8520 = DIRECTION ( 'NONE',  ( 0.000000000000000000, 0.000000000000000000, 1.000000000000000000 ) ) ;
#8521 =( BOUNDED_CURVE ( )  B_SPLINE_CURVE ( 2, ( #3346, #4332, #8309, #357, #8361, #8260, #5957, #5059, #4962 ),
 .UNSPECIFIED., .F., .T. ) 
 B_SPLINE_CURVE_WITH_KNOTS ( ( 3, 2, 2, 2, 3 ),
 ( 0.8125000000000000000, 0.8194444444444444198, 0.8333333333333333703, 0.8472222222222222099, 0.8541666666666667407 ),
 .UNSPECIFIED. ) 
 CURVE ( )  GEOMETRIC_REPRESENTATION_ITEM ( )  RATIONAL_B_SPLINE_CURVE ( ( 0.9330127018922194093, 0.9330127018922194093, 1.000000000000000000, 0.8660254037844387076, 1.000000000000000000, 0.8660254037844387076, 1.000000000000000000, 0.9330127018922187432, 0.9330127018922192983 ) ) 
 REPRESENTATION_ITEM ( '' )  );
#8522 = DIRECTION ( 'NONE',  ( -1.000000000000000000, 0.000000000000000000, 0.000000000000000000 ) ) ;
#8523 = ORIENTED_EDGE ( 'NONE', *, *, #9416, .T. ) ;
#8524 = B_SPLINE_CURVE_WITH_KNOTS ( 'NONE', 3,
 ( #1993, #9220, #8391, #1222, #2108, #4413, #7597, #10123, #2052, #2962, #7655 ),
 .UNSPECIFIED., .F., .F.,
 ( 4, 1, 1, 1, 1, 1, 1, 1, 4 ),
 ( 0.000000000000000000, 0.1199228846740813259, 0.2396820999030742083, 0.3587608595380448184, 0.4799620281296770319, 0.6043577515038436321, 0.7314057062717854718, 0.8632643124108332344, 1.000000000000000000 ),
 .UNSPECIFIED. ) ;
#8525 = CARTESIAN_POINT ( 'NONE',  ( -16.05932294508833280, 99.50000000000000000, 15.21084698918278555 ) ) ;
#8526 = CARTESIAN_POINT ( 'NONE',  ( -11.36312591709335962, 2.999999998907525445, -27.43301270000000258 ) ) ;
#8527 = ORIENTED_EDGE ( 'NONE', *, *, #1194, .T. ) ;
#8528 = CARTESIAN_POINT ( 'NONE',  ( -1.767625397874844694E-16, -1.912499999999999867, -2.886751345948128655 ) ) ;
#8529 = CARTESIAN_POINT ( 'NONE',  ( -22.67573144110267336, 99.50000000000001421, -10.14737752305977381 ) ) ;
#8530 = CYLINDRICAL_SURFACE ( 'NONE', #2929, 27.00000000000000355 ) ;
#8531 = CARTESIAN_POINT ( 'NONE',  ( 2.256430356250000102, -1.378124999385482941, -2.763330213280484622E-16 ) ) ;
#8532 = CARTESIAN_POINT ( 'NONE',  ( 4.871887406949175769, 99.49999999999995737, -23.77896509604281405 ) ) ;
#8533 = CARTESIAN_POINT ( 'NONE',  ( 19.39806930854667399, 1.849999998907525312, 19.39806930854668465 ) ) ;
#8534 = UNCERTAINTY_MEASURE_WITH_UNIT (LENGTH_MEASURE( 1.000000000000000082E-05 ), #9367, 'distance_accuracy_value', 'NONE');
#8535 = CARTESIAN_POINT ( 'NONE',  ( -15.69015368034045643, 100.0000000000000142, 16.64011368054243434 ) ) ;
#8536 = FACE_BOUND ( 'NONE', #934, .T. ) ;
#8537 = CARTESIAN_POINT ( 'NONE',  ( 2.847408871211157155, 99.50000000000001421, -22.10537533382872510 ) ) ;
#8538 = DIRECTION ( 'NONE',  ( 0.000000000000000000, 0.000000000000000000, 1.000000000000000000 ) ) ;
#8539 = VECTOR ( 'NONE', #9093, 1000.000000000000000 ) ;
#8540 = ORIENTED_EDGE ( 'NONE', *, *, #2242, .F. ) ;
#8541 = CARTESIAN_POINT ( 'NONE',  ( -2.256430356250000102, -2.390624999385482674, 0.000000000000000000 ) ) ;
#8542 = CARTESIAN_POINT ( 'NONE',  ( -21.20999280589743918, 99.50000000000002842, -11.35389291771566000 ) ) ;
#8543 = ORIENTED_EDGE ( 'NONE', *, *, #3832, .T. ) ;
#8544 = DIRECTION ( 'NONE',  ( 0.000000000000000000, 0.000000000000000000, 1.000000000000000000 ) ) ;
#8545 = CARTESIAN_POINT ( 'NONE',  ( -27.43301270000000258, 3.799999998907525711, -11.36312591709336317 ) ) ;
#8546 = FILL_AREA_STYLE ('',( #6858 ) ) ;
#8547 = DIRECTION ( 'NONE',  ( 4.336808689942017736E-16, 0.000000000000000000, -1.000000000000000000 ) ) ;
#8548 = APPLICATION_CONTEXT ( 'automotive_design' ) ;
#8549 = CARTESIAN_POINT ( 'NONE',  ( 27.00000000000000355, 1.600000000000000089, 0.000000000000000000 ) ) ;
#8550 = CARTESIAN_POINT ( 'NONE',  ( 8.684839681857363658, 99.50000000000001421, 19.94043386883836178 ) ) ;
#8551 = VERTEX_POINT ( 'NONE', #3182 ) ;
#8552 = CARTESIAN_POINT ( 'NONE',  ( -16.56356094049941419, 99.49999999999997158, 15.77213757552179629 ) ) ;
#8553 = CARTESIAN_POINT ( 'NONE',  ( 8.132491713109027742, 99.50000000000001421, 21.08089001807756446 ) ) ;
#8554 = VERTEX_POINT ( 'NONE', #7096 ) ;
#8555 = CARTESIAN_POINT ( 'NONE',  ( -1.128215178124998497, -1.978124999385482807, 1.954126010382872147 ) ) ;
#8556 = ORIENTED_EDGE ( 'NONE', *, *, #8315, .F. ) ;
#8557 = EDGE_LOOP ( 'NONE', ( #10169, #10082, #3266, #5934 ) ) ;
#8558 = EDGE_CURVE ( 'NONE', #8551, #9293, #6368, .T. ) ;
#8559 = CARTESIAN_POINT ( 'NONE',  ( -3.000000000000000888, -15.00000000000000000, -1.732050807568877415 ) ) ;
#8560 = CARTESIAN_POINT ( 'NONE',  ( 0.000000000000000000, 97.00000000000000000, -17.50000000000000355 ) ) ;
#8561 = CARTESIAN_POINT ( 'NONE',  ( 4.786228327491940187E-16, -2.390624999385482230, 2.605501347177161087 ) ) ;
#8562 = CARTESIAN_POINT ( 'NONE',  ( 4.922541232168287983, 100.0000000000000568, -24.37252920941159928 ) ) ;
#8563 = CARTESIAN_POINT ( 'NONE',  ( -2.500000000000000000, -1.800000000000000044, 0.000000000000000000 ) ) ;
#8564 = CARTESIAN_POINT ( 'NONE',  ( 4.358720771404392735, 99.50000000000000000, -21.20742720589606378 ) ) ;
#8565 = ORIENTED_EDGE ( 'NONE', *, *, #5503, .T. ) ;
#8566 = EDGE_CURVE ( 'NONE', #6757, #26, #1601, .T. ) ;
#8567 = CARTESIAN_POINT ( 'NONE',  ( 3.411785164761435674, 99.50000000000000000, -22.76693382491622231 ) ) ;
#8568 = CARTESIAN_POINT ( 'NONE',  ( 27.00000000000000355, 0.8000000000000000444, 0.000000000000000000 ) ) ;
#8569 = ORIENTED_EDGE ( 'NONE', *, *, #8887, .T. ) ;
#8570 = CARTESIAN_POINT ( 'NONE',  ( 1.250000000000001110, -1.199999999999999956, 2.165063509461096380 ) ) ;
#8571 = LINE ( 'NONE', #3033, #4539 ) ;
#8572 = CARTESIAN_POINT ( 'NONE',  ( 2.256430356250000546, -0.4031249993854829627, 1.302750673588579877 ) ) ;
#8573 = VECTOR ( 'NONE', #3427, 1000.000000000000227 ) ;
#8574 = EDGE_LOOP ( 'NONE', ( #4101, #2800, #7377, #4460 ) ) ;
#8575 = CARTESIAN_POINT ( 'NONE',  ( -22.05573893622344173, 100.0000000000000000, -9.391591294897233766 ) ) ;
#8576 = CARTESIAN_POINT ( 'NONE',  ( 4.772556553149396308, 99.49999999999997158, -24.49721679606612312 ) ) ;
#8577 = EDGE_CURVE ( 'NONE', #519, #776, #1024, .T. ) ;
#8578 = CARTESIAN_POINT ( 'NONE',  ( 4.996790860652426159E-15, -1.912499999999999867, -2.500000000000000000 ) ) ;
#8579 = CARTESIAN_POINT ( 'NONE',  ( -16.57330815294036697, 99.50000000000001421, 15.84440382193293217 ) ) ;
#8580 = VECTOR ( 'NONE', #419, 1000.000000000000114 ) ;
#8581 = VERTEX_POINT ( 'NONE', #1839 ) ;
#8582 = EDGE_CURVE ( 'NONE', #7789, #8960, #2544, .T. ) ;
#8583 = CARTESIAN_POINT ( 'NONE',  ( 24.91446314102564230, 100.0000000000000000, -1.581029647435897578 ) ) ;
#8584 =( GEOMETRIC_REPRESENTATION_CONTEXT ( 3 ) GLOBAL_UNCERTAINTY_ASSIGNED_CONTEXT ( ( #10098 ) ) GLOBAL_UNIT_ASSIGNED_CONTEXT ( ( #1933, #1104, #374 ) ) REPRESENTATION_CONTEXT ( 'NONE', 'WORKASPACE' ) );
#8585 = CARTESIAN_POINT ( 'NONE',  ( 27.43301270000000258, 1.949999998907525178, 0.000000000000000000 ) ) ;
#8586 = ORIENTED_EDGE ( 'NONE', *, *, #699, .F. ) ;
#8587 = CARTESIAN_POINT ( 'NONE',  ( -2.500000000000000000, -3.187499999999999556, -1.443375672974064106 ) ) ;
#8588 = CARTESIAN_POINT ( 'NONE',  ( 0.000000000000000000, 0.000000000000000000, 0.000000000000000000 ) ) ;
#8589 = CARTESIAN_POINT ( 'NONE',  ( -22.08823018108446234, 100.0000000000000000, -9.406177930363766038 ) ) ;
#8590 = CARTESIAN_POINT ( 'NONE',  ( -1.128215178125000273, -1.678124999385482763, -1.954126010382871259 ) ) ;
#8591 = CARTESIAN_POINT ( 'NONE',  ( -20.93575003794465061, 99.50000000000001421, -10.12220034237898503 ) ) ;
#8592 = CARTESIAN_POINT ( 'NONE',  ( -11.36312591709335962, 1.399999998907525578, -27.43301270000000258 ) ) ;
#8594 = ORIENTED_EDGE ( 'NONE', *, *, #2386, .T. ) ;
#8593 = ORIENTED_EDGE ( 'NONE', *, *, #3187, .T. ) ;
#8595 = CARTESIAN_POINT ( 'NONE',  ( -15.56505537928961047, 100.0000000000000284, 14.87309967080592088 ) ) ;
#8596 = DIRECTION ( 'NONE',  ( -0.000000000000000000, -1.000000000000000000, -0.000000000000000000 ) ) ;
#8597 = CARTESIAN_POINT ( 'NONE',  ( 3.207057600658871355, 99.50000000000000000, -22.07913334414698880 ) ) ;
#8598 = ADVANCED_FACE ( 'NONE', ( #138 ), #280, .F. ) ;
#8599 = CARTESIAN_POINT ( 'NONE',  ( -15.32348647777738826, 100.0000000000000000, 15.39505148541300450 ) ) ;
#8600 = EDGE_LOOP ( 'NONE', ( #7792, #3904, #7868, #3572 ) ) ;
#8601 = CARTESIAN_POINT ( 'NONE',  ( 1.128215178124999607, -0.7406249993854829849, -1.954126010382871259 ) ) ;
#8602 = CARTESIAN_POINT ( 'NONE',  ( 4.743081672682207817, 99.50000000000002842, -21.60795120912350598 ) ) ;
#8603 = VERTEX_POINT ( 'NONE', #7492 ) ;
#8604 = CARTESIAN_POINT ( 'NONE',  ( 1.128215178125001161, -2.240624999385482763, 1.954126010382870815 ) ) ;
#8605 = CARTESIAN_POINT ( 'NONE',  ( 1.679787559701184688E-15, 2.849999998907525534, -27.43301270000000258 ) ) ;
#8606 = ORIENTED_EDGE ( 'NONE', *, *, #7579, .F. ) ;
#8607 = CARTESIAN_POINT ( 'NONE',  ( 4.486604876299897349, 99.50000000000000000, -21.85617661337775885 ) ) ;
#8608 = DIRECTION ( 'NONE',  ( -0.000000000000000000, 1.000000000000000000, -0.000000000000000000 ) ) ;
#8609 = EDGE_LOOP ( 'NONE', ( #1743, #857 ) ) ;
#8610 = CARTESIAN_POINT ( 'NONE',  ( -15.19031985176477662, 99.49999999999998579, 15.56880617076518547 ) ) ;
#8611 = CARTESIAN_POINT ( 'NONE',  ( 8.091962505948220752, 99.49999999999995737, 20.48385654212622242 ) ) ;
#8612 = CARTESIAN_POINT ( 'NONE',  ( 2.256430356250000102, -3.178124999385482319, -2.763330213280484622E-16 ) ) ;
#8613 = ORIENTED_EDGE ( 'NONE', *, *, #9416, .F. ) ;
#8614 = EDGE_LOOP ( 'NONE', ( #4150, #10285, #5269, #1001 ) ) ;
#8615 = DIRECTION ( 'NONE',  ( 0.000000000000000000, -0.000000000000000000, 1.000000000000000000 ) ) ;
#8616 = CARTESIAN_POINT ( 'NONE',  ( -21.73488407773357167, 99.50000000000000000, -9.647150398373231184 ) ) ;
#8617 = B_SPLINE_SURFACE_WITH_KNOTS ( 'NONE', 3, 1, ( 
 ( #6714, #9501 ),
 ( #9965, #1378 ),
 ( #7029, #6246 ),
 ( #5420, #9333 ),
 ( #7766, #6137 ),
 ( #3014, #4363 ),
 ( #7081, #337 ),
 ( #8552, #3894 ),
 ( #5363, #3792 ),
 ( #4627, #6977 ),
 ( #2325, #649 ),
 ( #7869, #10286 ),
 ( #3120, #10178 ),
 ( #2744, #4313 ),
 ( #2276, #5936 ),
 ( #5472, #8663 ),
 ( #1486, #5674 ),
 ( #7973, #9592 ),
 ( #907, #4926 ) ),
 .UNSPECIFIED., .F., .F., .F.,
 ( 4, 1, 1, 1, 1, 1, 1, 1, 1, 1, 1, 1, 1, 1, 1, 1, 4 ),
 ( 2, 2 ),
 ( 0.000000000000000000, 0.06442465027149940626, 0.1272622498775801414, 0.1890519169419207224, 0.2498421757728049863, 0.3110425729590077792, 0.3720985300252119266, 0.4351465435385043490, 0.5001170788027262670, 0.5644817420234762295, 0.6276143074669133792, 0.6889588046791949028, 0.7501592018653976401, 0.8106582772613761811, 0.8724479443257179279, 0.9351683423010851426, 1.000000000000000000 ),
 ( 0.000000000000000000, 1.000000000000000000 ),
 .UNSPECIFIED. ) ;
#8618 = CARTESIAN_POINT ( 'NONE',  ( -1.595409442497313560E-16, -0.8156249993854828295, -2.605501347177161087 ) ) ;
#8619 = CARTESIAN_POINT ( 'NONE',  ( 3.124251205490514494, 100.0000000000000000, -23.02140944421609703 ) ) ;
#8620 = EDGE_CURVE ( 'NONE', #4631, #4436, #3473, .T. ) ;
#8621 = DIRECTION ( 'NONE',  ( 0.000000000000000000, 0.000000000000000000, 1.000000000000000000 ) ) ;
#8622 = CARTESIAN_POINT ( 'NONE',  ( -1.767625397874844694E-16, -2.306249998770966148, -2.886751345948128655 ) ) ;
#8623 = ORIENTED_EDGE ( 'NONE', *, *, #6274, .T. ) ;
#8624 = AXIS2_PLACEMENT_3D ( 'NONE', #4129, #5049, #8250 ) ;
#8625 = CARTESIAN_POINT ( 'NONE',  ( 3.080354370726382296, 99.50000000000004263, -23.09295995363041598 ) ) ;
#8626 = CARTESIAN_POINT ( 'NONE',  ( 9.575551604960836016, 100.0000000000000142, 20.57049984249936969 ) ) ;
#8627 = ORIENTED_EDGE ( 'NONE', *, *, #7517, .F. ) ;
#8628 = CARTESIAN_POINT ( 'NONE',  ( 4.486604876299897349, 100.0000000000000000, -21.85617661337775885 ) ) ;
#8629 = CARTESIAN_POINT ( 'NONE',  ( -2.256430356249999214, -0.5531249993854828739, 1.302750673588581876 ) ) ;
#8630 = EDGE_CURVE ( 'NONE', #6174, #9675, #1667, .T. ) ;
#8631 = EDGE_LOOP ( 'NONE', ( #7247, #137, #5483, #70 ) ) ;
#8632 = CARTESIAN_POINT ( 'NONE',  ( 1.662111305799679408E-15, 5.516666664845875090, -27.14433756666667108 ) ) ;
#8633 = CARTESIAN_POINT ( 'NONE',  ( 4.922541232168287983, 99.50000000000002842, -24.37252920941159928 ) ) ;
#8634 =( LENGTH_UNIT ( ) NAMED_UNIT ( * ) SI_UNIT ( .MILLI., .METRE. ) );
#8635 = AXIS2_PLACEMENT_3D ( 'NONE', #9215, #3514, #2786 ) ;
#8636 = CARTESIAN_POINT ( 'NONE',  ( -1.249999999999998224, -3.468749998770965348, 2.165063509461097713 ) ) ;
#8637 = VERTEX_POINT ( 'NONE', #6515 ) ;
#8638 = CARTESIAN_POINT ( 'NONE',  ( -15.91768310440539658, 100.0000000000000284, 15.18344740530786652 ) ) ;
#8639 = CARTESIAN_POINT ( 'NONE',  ( -27.43301270000000969, 1.599999998907525756, 11.36312591709335784 ) ) ;
#8640 = VERTEX_POINT ( 'NONE', #9904 ) ;
#8641 = LINE ( 'NONE', #8842, #8756 ) ;
#8642 = DIRECTION ( 'NONE',  ( 0.2907756355032780071, 0.000000000000000000, 0.9567912676219745283 ) ) ;
#8643 = CARTESIAN_POINT ( 'NONE',  ( 2.256430356249999658, -1.340624999385482852, -1.302750673588581432 ) ) ;
#8644 = CARTESIAN_POINT ( 'NONE',  ( -16.63177974700816009, 99.50000000000000000, 16.59747536361813403 ) ) ;
#8645 = CARTESIAN_POINT ( 'NONE',  ( -5.039362679103552881E-15, 3.349999998907525534, 27.43301270000000258 ) ) ;
#8646 = UNCERTAINTY_MEASURE_WITH_UNIT (LENGTH_MEASURE( 1.000000000000000082E-05 ), #7893, 'distance_accuracy_value', 'NONE');
#8647 = CARTESIAN_POINT ( 'NONE',  ( -15.27171031718473770, 100.0000000000000000, 15.44886715306589764 ) ) ;
#8648 = CARTESIAN_POINT ( 'NONE',  ( 3.888553205800344248, 99.49999999999995737, -24.35333287445124739 ) ) ;
#8649 = CARTESIAN_POINT ( 'NONE',  ( 3.317038232150706367, 99.49999999999998579, -21.66195598387956878 ) ) ;
#8650 = CARTESIAN_POINT ( 'NONE',  ( -19.46743691185369585, 99.50000000000000000, -8.912588186774021537 ) ) ;
#8651 = VECTOR ( 'NONE', #9174, 1000.000000000000227 ) ;
#8652 = CARTESIAN_POINT ( 'NONE',  ( 2.256430356250000102, -0.3656249993854829294, -2.763330213280484622E-16 ) ) ;
#8653 = CARTESIAN_POINT ( 'NONE',  ( 4.200543313440712190, 99.50000000000000000, -21.13206004899810608 ) ) ;
#8654 = VERTEX_POINT ( 'NONE', #2739 ) ;
#8655 = CARTESIAN_POINT ( 'NONE',  ( 2.256430356250000102, -1.715624999385482852, -2.763330213280484622E-16 ) ) ;
#8656 = CARTESIAN_POINT ( 'NONE',  ( 27.43301269999999548, 3.399999998907525356, 11.36312591709337738 ) ) ;
#8657 = ADVANCED_FACE ( 'NONE', ( #3368 ), #923, .T. ) ;
#8658 = DIRECTION ( 'NONE',  ( -0.000000000000000000, -1.000000000000000000, 0.000000000000000000 ) ) ;
#8659 = EDGE_CURVE ( 'NONE', #1908, #8324, #9966, .T. ) ;
#8660 = CARTESIAN_POINT ( 'NONE',  ( -27.00000000000001421, 1.250000000000000222, 11.18376618407356382 ) ) ;
#8661 = CARTESIAN_POINT ( 'NONE',  ( -20.96643530928959365, 99.99999999999997158, -10.05541671241504886 ) ) ;
#8662 = ORIENTED_EDGE ( 'NONE', *, *, #4290, .F. ) ;
#8663 = CARTESIAN_POINT ( 'NONE',  ( -16.45391695211397831, 100.0000000000000000, 16.32580124622701589 ) ) ;
#8664 = CARTESIAN_POINT ( 'NONE',  ( 8.281567445270807681, 99.50000000000000000, 20.15885744430370252 ) ) ;
#8665 = ORIENTED_EDGE ( 'NONE', *, *, #2814, .F. ) ;
#8666 = CARTESIAN_POINT ( 'NONE',  ( -2.256430356250000102, -4.790624999385483029, -1.302750673588580321 ) ) ;
#8667 = ORIENTED_EDGE ( 'NONE', *, *, #6377, .F. ) ;
#8668 = EDGE_LOOP ( 'NONE', ( #7458, #5613, #8527, #3548 ) ) ;
#8669 = CARTESIAN_POINT ( 'NONE',  ( -27.43301270000000969, 3.899999998907525356, 11.36312591709335784 ) ) ;
#8670 = FACE_OUTER_BOUND ( 'NONE', #6446, .T. ) ;
#8671 = CARTESIAN_POINT ( 'NONE',  ( 1.128215178125001161, -1.903124999385482852, 1.954126010382870815 ) ) ;
#8672 = CARTESIAN_POINT ( 'NONE',  ( -27.00000000000000355, 3.600000000000000533, -3.306546357697854128E-15 ) ) ;
#8673 = CARTESIAN_POINT ( 'NONE',  ( 27.00000000000000355, 4.599999997815050534, 0.000000000000000000 ) ) ;
#8674 = AXIS2_PLACEMENT_3D ( 'NONE', #6689, #9004, #5068 ) ;
#8675 = CARTESIAN_POINT ( 'NONE',  ( 2.500000000000000444, -2.006249998770965437, 1.443375672974063439 ) ) ;
#8676 = CARTESIAN_POINT ( 'NONE',  ( 9.877377282685029372E-16, -1.181249998770965703, 2.500000000000000000 ) ) ;
#8677 = CARTESIAN_POINT ( 'NONE',  ( -20.72805389903318130, 99.50000000000000000, -9.848585782927868237 ) ) ;
#8678 = ORIENTED_EDGE ( 'NONE', *, *, #6951, .T. ) ;
#8679 = CARTESIAN_POINT ( 'NONE',  ( 2.500000000000000000, -4.237499999999999822, -1.443375672974065438 ) ) ;
#8680 = CARTESIAN_POINT ( 'NONE',  ( 4.786228327491941173E-16, -0.4781249993854829183, 2.605501347177161087 ) ) ;
#8681 = ORIENTED_EDGE ( 'NONE', *, *, #5491, .T. ) ;
#8682 = CARTESIAN_POINT ( 'NONE',  ( 2.958578797724396026, 99.50000000000000000, -23.36432507653281121 ) ) ;
#8683 = CARTESIAN_POINT ( 'NONE',  ( 9.778118981323553172, 99.99999999999998579, 20.11889122584574352 ) ) ;
#8684 =( BOUNDED_CURVE ( )  B_SPLINE_CURVE ( 2, ( #1723, #2358, #5555, #6287, #8112, #4083, #8748, #942, #5659 ),
 .UNSPECIFIED., .F., .F. ) 
 B_SPLINE_CURVE_WITH_KNOTS ( ( 3, 2, 2, 2, 3 ),
 ( 0.5357142857142856984, 0.5535714285714286031, 0.5714285714285713969, 0.5892857142857143016, 0.6071428571428570953 ),
 .UNSPECIFIED. ) 
 CURVE ( )  GEOMETRIC_REPRESENTATION_ITEM ( )  RATIONAL_B_SPLINE_CURVE ( ( 1.000000000000000000, 0.9238795325112867385, 1.000000000000000000, 0.9238795325112867385, 1.000000000000000000, 0.9238795325112867385, 1.000000000000000000, 0.9238795325112867385, 1.000000000000000000 ) ) 
 REPRESENTATION_ITEM ( '' )  );
#8685 = CARTESIAN_POINT ( 'NONE',  ( -1.728530063377412329, -5.141148402510967941, -1.450400555903694766 ) ) ;
#8686 = CARTESIAN_POINT ( 'NONE',  ( -16.36254897777739004, 99.50000000000001421, 15.39785597259249350 ) ) ;
#8687 = ORIENTED_EDGE ( 'NONE', *, *, #4224, .T. ) ;
#8688 = CARTESIAN_POINT ( 'NONE',  ( 1.653273178848927064E-15, 3.199999997815050623, -27.00000000000000355 ) ) ;
#8689 = CARTESIAN_POINT ( 'NONE',  ( -27.43301270000000258, 4.749999998907525445, -3.359575119402369376E-15 ) ) ;
#8690 = ORIENTED_EDGE ( 'NONE', *, *, #2685, .F. ) ;
#8691 = EDGE_CURVE ( 'NONE', #9173, #8491, #231, .T. ) ;
#8692 = CARTESIAN_POINT ( 'NONE',  ( -1.767625397874844694E-16, -4.612499999999998934, -2.886751345948128655 ) ) ;
#8693 = CONTEXT_DEPENDENT_SHAPE_REPRESENTATION ( #9075, #6440 ) ;
#8694 = CARTESIAN_POINT ( 'NONE',  ( 3.291601991079349698, 99.99999999999997158, -22.28586332678438353 ) ) ;
#8695 = CARTESIAN_POINT ( 'NONE',  ( 2.256430356249999658, -4.490624999385483207, -1.302750673588581432 ) ) ;
#8696 = CARTESIAN_POINT ( 'NONE',  ( -16.67860655220511035, 99.49999999999998579, 15.23428378554110374 ) ) ;
#8697 = CARTESIAN_POINT ( 'NONE',  ( 27.00000000000000355, 1.399999997815050579, 0.000000000000000000 ) ) ;
#8698 = CARTESIAN_POINT ( 'NONE',  ( 4.486604876299897349, 100.0000000000000000, -21.85617661337775885 ) ) ;
#8699 = LINE ( 'NONE', #1637, #6326 ) ;
#8700 = CARTESIAN_POINT ( 'NONE',  ( 3.204253864046738176, 99.50000000000000000, -22.06071064728738662 ) ) ;
#8701 = B_SPLINE_SURFACE_WITH_KNOTS ( 'NONE', 3, 1, ( 
 ( #8058, #1519 ),
 ( #5605, #684 ),
 ( #842, #739 ),
 ( #4665, #4034 ),
 ( #3297, #6385 ),
 ( #892, #5554 ),
 ( #4082, #7170 ),
 ( #6487, #7215 ),
 ( #8747, #7854 ),
 ( #51, #2256 ),
 ( #3156, #7264 ),
 ( #4761, #9578 ),
 ( #2462, #4713 ),
 ( #2126, #2357 ),
 ( #106, #6286 ),
 ( #5458, #2410 ),
 ( #7064, #8647 ),
 ( #5509, #10271 ),
 ( #1674, #3876 ) ),
 .UNSPECIFIED., .F., .F., .F.,
 ( 4, 1, 1, 1, 1, 1, 1, 1, 1, 1, 1, 1, 1, 1, 1, 1, 4 ),
 ( 2, 2 ),
 ( 0.000000000000000000, 0.06473908249738200005, 0.1274869542813800993, 0.1888754624962200035, 0.2498352098569301405, 0.3101749858420705941, 0.3718734486855839183, 0.4342313324889700565, 0.4990836447755341299, 0.5639614065304963120, 0.6264045329497629488, 0.6882484937299673255, 0.7493615009078817835, 0.8100377551054726011, 0.8717391907241844873, 0.9348513958286107650, 1.000000000000000000 ),
 ( 0.000000000000000000, 1.000000000000000000 ),
 .UNSPECIFIED. ) ;
#8702 = PLANE ( 'NONE',  #8295 ) ;
#8703 = CARTESIAN_POINT ( 'NONE',  ( 1.128215178125001161, -2.690624999385482941, 1.954126010382870815 ) ) ;
#8704 = CARTESIAN_POINT ( 'NONE',  ( -20.72805389903318130, 99.50000000000000000, -9.848585782927868237 ) ) ;
#8705 = ORIENTED_EDGE ( 'NONE', *, *, #5584, .F. ) ;
#8706 = ADVANCED_FACE ( 'NONE', ( #4162 ), #495, .T. ) ;
#8707 = EDGE_LOOP ( 'NONE', ( #8499, #9934, #4205, #3967, #1965, #3633 ) ) ;
#8708 = CARTESIAN_POINT ( 'NONE',  ( 4.786228327491941173E-16, -2.278124999385482852, 2.605501347177161087 ) ) ;
#8709 = CARTESIAN_POINT ( 'NONE',  ( 1.679787559701184688E-15, 0.5499999989075251561, -27.43301270000000258 ) ) ;
#8710 = CARTESIAN_POINT ( 'NONE',  ( -15.09818093130665773, 99.50000000000000000, 16.69478731934044191 ) ) ;
#8711 = CARTESIAN_POINT ( 'NONE',  ( 19.09188309203678813, 0.1000000000000000056, -19.09188309203678813 ) ) ;
#8712 = CARTESIAN_POINT ( 'NONE',  ( -2.562556682370380035, -20.00000000000000000, 1.479492790380213751 ) ) ;
#8713 = PRODUCT_DEFINITION ( 'UNKNOWN', '', #3812, #7062 ) ;
#8714 = CYLINDRICAL_SURFACE ( 'NONE', #3472, 2.500000000000000000 ) ;
#8715 = CARTESIAN_POINT ( 'NONE',  ( -15.42956291708403782, 99.99999999999998579, 16.53061251458192515 ) ) ;
#8716 = EDGE_CURVE ( 'NONE', #6863, #2532, #7544, .T. ) ;
#8717 = CARTESIAN_POINT ( 'NONE',  ( -1.128215178124998497, -5.128124999385482496, 1.954126010382872147 ) ) ;
#8718 = DIRECTION ( 'NONE',  ( -0.9197984731044490658, 0.000000000000000000, 0.3923910917372159246 ) ) ;
#8719 = EDGE_CURVE ( 'NONE', #3650, #4452, #3741, .T. ) ;
#8720 = CARTESIAN_POINT ( 'NONE',  ( 11.36312591709336139, 1.999999998907525445, -27.43301270000000258 ) ) ;
#8721 = CARTESIAN_POINT ( 'NONE',  ( 3.824506687597884369, 100.0000000000000284, -24.68145443631992109 ) ) ;
#8722 = CARTESIAN_POINT ( 'NONE',  ( 4.786228327491940187E-16, -0.5906249993854828517, 2.605501347177161087 ) ) ;
#8723 = LINE ( 'NONE', #10347, #1201 ) ;
#8724 = FACE_OUTER_BOUND ( 'NONE', #7389, .T. ) ;
#8725 = CARTESIAN_POINT ( 'NONE',  ( 4.446585460023182890, 99.50000000000002842, -21.79057454014859019 ) ) ;
#8726 = EDGE_LOOP ( 'NONE', ( #1526, #278, #4100, #5789, #1023, #4459, #2879, #6251, #5437, #7650, #1803, #1791, #3921, #6293, #180, #7101, #8140 ) ) ;
#8727 = CARTESIAN_POINT ( 'NONE',  ( 1.249999999999999334, -1.893749998770965837, -2.165063509461096825 ) ) ;
#8728 = ORIENTED_EDGE ( 'NONE', *, *, #2179, .T. ) ;
#8729 = LINE ( 'NONE', #2290, #5792 ) ;
#8730 = CARTESIAN_POINT ( 'NONE',  ( 9.877377282685029372E-16, -3.037499999999999201, 2.500000000000000000 ) ) ;
#8731 = CARTESIAN_POINT ( 'NONE',  ( 8.857094148306096315, 99.50000000000001421, 19.57755665027156766 ) ) ;
#8732 = CARTESIAN_POINT ( 'NONE',  ( -2.256430356250000102, -4.190624999385482496, 0.000000000000000000 ) ) ;
#8733 = CONICAL_SURFACE ( 'NONE', #9881, 2.500000000000000444, 0.08726646259971666819 ) ;
#8734 = CARTESIAN_POINT ( 'NONE',  ( -22.28244091826395135, 100.0000000000000000, -10.68852969318427881 ) ) ;
#8735 =( NAMED_UNIT ( * ) SI_UNIT ( $, .STERADIAN. ) SOLID_ANGLE_UNIT ( ) );
#8736 = CARTESIAN_POINT ( 'NONE',  ( -22.28244091826395135, 99.50000000000000000, -10.68852969318427881 ) ) ;
#8737 = CARTESIAN_POINT ( 'NONE',  ( -14.83571502646304197, 99.50000000000004263, 16.32397075880403392 ) ) ;
#8738 = CARTESIAN_POINT ( 'NONE',  ( 19.39806930854668110, 4.449999998907525622, -19.39806930854668110 ) ) ;
#8739 = VECTOR ( 'NONE', #4050, 1000.000000000000000 ) ;
#8740 = EDGE_LOOP ( 'NONE', ( #1316, #4531, #3068, #2995 ) ) ;
#8741 = CARTESIAN_POINT ( 'NONE',  ( -1.767625397874844694E-16, -3.262499999999999289, -2.886751345948128655 ) ) ;
#8742 = CARTESIAN_POINT ( 'NONE',  ( 3.986298408513477387, 100.0000000000000284, -22.53092616755505162 ) ) ;
#8743 = CARTESIAN_POINT ( 'NONE',  ( 4.786228327491941173E-16, -3.290624999385482585, 2.605501347177161087 ) ) ;
#8744 = CARTESIAN_POINT ( 'NONE',  ( -20.45905772418405988, 99.50000000000000000, -10.59533404166311321 ) ) ;
#8745 = CARTESIAN_POINT ( 'NONE',  ( 19.39806930854667399, 4.249999998907525445, 19.39806930854668465 ) ) ;
#8746 = EDGE_CURVE ( 'NONE', #2748, #9210, #8524, .T. ) ;
#8747 = CARTESIAN_POINT ( 'NONE',  ( -15.10617644529808423, 99.50000000000002842, 15.98944417891004477 ) ) ;
#8748 = CARTESIAN_POINT ( 'NONE',  ( 19.09188309203678813, 3.899999997815050357, -19.09188309203678813 ) ) ;
#8749 = CARTESIAN_POINT ( 'NONE',  ( 3.207057600658871355, 100.0000000000000000, -22.07913334414698880 ) ) ;
#8750 = FACE_OUTER_BOUND ( 'NONE', #149, .T. ) ;
#8751 = CARTESIAN_POINT ( 'NONE',  ( 2.256430356250000102, -3.965624999385482408, -2.763330213280484622E-16 ) ) ;
#8752 = LINE ( 'NONE', #3835, #6469 ) ;
#8753 = CARTESIAN_POINT ( 'NONE',  ( -2.256430356250000102, -2.390624999385482674, 0.000000000000000000 ) ) ;
#8754 = CARTESIAN_POINT ( 'NONE',  ( 19.39806930854667399, 1.049999998907525045, 19.39806930854668465 ) ) ;
#8755 = CARTESIAN_POINT ( 'NONE',  ( -15.15193744131588183, 99.50000000000001421, 16.74589488344418697 ) ) ;
#8756 = VECTOR ( 'NONE', #4173, 1000.000000000000000 ) ;
#8757 = CARTESIAN_POINT ( 'NONE',  ( -11.18376618407356560, 4.250000000000000888, -27.00000000000000355 ) ) ;
#8758 = CARTESIAN_POINT ( 'NONE',  ( -3.486133158594716510E-16, -4.106249998770965526, -2.500000000000000000 ) ) ;
#8759 = ADVANCED_FACE ( 'NONE', ( #435 ), #1329, .F. ) ;
#8760 = CARTESIAN_POINT ( 'NONE',  ( 0.000000000000000000, 105.0000000000000142, 0.000000000000000000 ) ) ;
#8761 = CARTESIAN_POINT ( 'NONE',  ( 8.540544597724410991, 99.50000000000000000, 19.98924338346217766 ) ) ;
#8762 = ORIENTED_EDGE ( 'NONE', *, *, #7643, .F. ) ;
#8763 = FACE_OUTER_BOUND ( 'NONE', #5303, .T. ) ;
#8764 = VERTEX_POINT ( 'NONE', #492 ) ;
#8765 = CARTESIAN_POINT ( 'NONE',  ( -27.43301270000000969, 2.299999998907525267, 11.36312591709335784 ) ) ;
#8766 = CARTESIAN_POINT ( 'NONE',  ( -19.09188309203678457, 1.899999999999999911, -19.09188309203678813 ) ) ;
#8767 = CARTESIAN_POINT ( 'NONE',  ( -27.00000000000000355, 0.9499999978150504010, -11.18376618407357270 ) ) ;
#8768 = CARTESIAN_POINT ( 'NONE',  ( 2.256430356249999658, -3.140624999385482674, -1.302750673588581432 ) ) ;
#8769 = DIRECTION ( 'NONE',  ( 0.9569724629708533659, 0.000000000000000000, -0.2901787468363226097 ) ) ;
#8770 = CARTESIAN_POINT ( 'NONE',  ( -22.67573144110267336, 99.50000000000001421, -10.14737752305977381 ) ) ;
#8771 = CARTESIAN_POINT ( 'NONE',  ( 8.074269155311188939, 100.0000000000000142, 20.56111086218762551 ) ) ;
#8772 = EDGE_LOOP ( 'NONE', ( #1865, #4796, #8780, #714 ) ) ;
#8773 = CARTESIAN_POINT ( 'NONE',  ( -2.500000000000000000, -1.743749998770965925, 0.000000000000000000 ) ) ;
#8774 = ORIENTED_EDGE ( 'NONE', *, *, #1641, .T. ) ;
#8775 = CARTESIAN_POINT ( 'NONE',  ( 4.584380863705032283, 100.0000000000000284, -24.21384527865288305 ) ) ;
#8776 = DIRECTION ( 'NONE',  ( 1.000000000000000000, 0.000000000000000000, 0.000000000000000000 ) ) ;
#8777 = CARTESIAN_POINT ( 'NONE',  ( 10.72103337977569204, 99.50000000000000000, 22.20268488987243316 ) ) ;
#8778 = CARTESIAN_POINT ( 'NONE',  ( 4.786228327491941173E-16, -3.628124999385482941, 2.605501347177161087 ) ) ;
#8779 = PRODUCT ( 'lid', 'lid', '', ( #411 ) ) ;
#8780 = ORIENTED_EDGE ( 'NONE', *, *, #5107, .F. ) ;
#8781 = EDGE_CURVE ( 'NONE', #2765, #3016, #8501, .T. ) ;
#8782 = CARTESIAN_POINT ( 'NONE',  ( 2.940192896829773250, 99.50000000000001421, -23.44521981770616037 ) ) ;
#8783 = CIRCLE ( 'NONE', #1079, 2.500000000000000444 ) ;
#8784 = DIRECTION ( 'NONE',  ( -0.000000000000000000, -1.000000000000000000, -0.000000000000000000 ) ) ;
#8785 = CARTESIAN_POINT ( 'NONE',  ( 2.500000000000000000, -1.931249998770965481, -1.443375672974065438 ) ) ;
#8786 = CARTESIAN_POINT ( 'NONE',  ( -14.74935495356232984, 99.50000000000001421, 15.91322402822111926 ) ) ;
#8787 = LINE ( 'NONE', #7951, #5642 ) ;
#8788 = VERTEX_POINT ( 'NONE', #548 ) ;
#8789 = CARTESIAN_POINT ( 'NONE',  ( 5.302876193624534821E-16, -4.387500000000000178, 2.886751345948128655 ) ) ;
#8790 = AXIS2_PLACEMENT_3D ( 'NONE', #6325, #7204, #4853 ) ;
#8791 = CARTESIAN_POINT ( 'NONE',  ( -2.500000000000000000, -0.3937499987709658922, 0.000000000000000000 ) ) ;
#8792 = CARTESIAN_POINT ( 'NONE',  ( -2.256430356249999214, -5.165624999385481253, 1.302750673588581876 ) ) ;
#8793 = CYLINDRICAL_SURFACE ( 'NONE', #9272, 2.500000000000000000 ) ;
#8794 = CARTESIAN_POINT ( 'NONE',  ( 11.18376618407357626, 2.049999997815050268, 27.00000000000000000 ) ) ;
#8795 = AXIS2_PLACEMENT_3D ( 'NONE', #5237, #4301, #7649 ) ;
#8796 = CARTESIAN_POINT ( 'NONE',  ( -20.64578974631102426, 99.49999999999995737, -10.10077944494247504 ) ) ;
#8797 = CARTESIAN_POINT ( 'NONE',  ( 0.000000000000000000, 105.0000000000000142, 0.000000000000000000 ) ) ;
#8798 = CARTESIAN_POINT ( 'NONE',  ( 3.214822648120007731, 100.0000000000000000, -21.86319392453323829 ) ) ;
#8799 = CARTESIAN_POINT ( 'NONE',  ( -2.256430356249998770, -4.603124999385482141, 1.302750673588581876 ) ) ;
#8800 = CARTESIAN_POINT ( 'NONE',  ( 4.143207896384923039, 99.49999999999998579, -24.36264353342416911 ) ) ;
#8801 = ORIENTED_EDGE ( 'NONE', *, *, #6274, .F. ) ;
#8802 = CARTESIAN_POINT ( 'NONE',  ( 1.128215178125001161, -3.140624999385482674, 1.954126010382870815 ) ) ;
#8803 = CARTESIAN_POINT ( 'NONE',  ( 19.39806930854668110, 2.049999998907525711, -19.39806930854668110 ) ) ;
#8804 =( NAMED_UNIT ( * ) PLANE_ANGLE_UNIT ( ) SI_UNIT ( $, .RADIAN. ) );
#8805 = CARTESIAN_POINT ( 'NONE',  ( 1.679787559701184688E-15, 5.349999998907525089, -27.43301270000000258 ) ) ;
#8806 = CARTESIAN_POINT ( 'NONE',  ( 11.18376618407357626, 3.850000000000000089, 27.00000000000000000 ) ) ;
#8807 = CARTESIAN_POINT ( 'NONE',  ( 0.000000000000000000, 97.00000000000000000, 0.000000000000000000 ) ) ;
#8808 = ORIENTED_EDGE ( 'NONE', *, *, #4146, .F. ) ;
#8809 = VECTOR ( 'NONE', #10012, 1000.000000000000000 ) ;
#8810 = FACE_OUTER_BOUND ( 'NONE', #3092, .T. ) ;
#8811 = CARTESIAN_POINT ( 'NONE',  ( -20.93575003794465061, 99.50000000000001421, -10.12220034237898503 ) ) ;
#8812 = CARTESIAN_POINT ( 'NONE',  ( 4.739008722453744049, 100.0000000000000142, -24.06821587619827696 ) ) ;
#8813 = VERTEX_POINT ( 'NONE', #6141 ) ;
#8814 = CLOSED_SHELL ( 'NONE', ( #7171, #995, #1087, #1673 ) ) ;
#8815 = CARTESIAN_POINT ( 'NONE',  ( -5.039362679103552881E-15, 3.249999998907525001, 27.43301270000000258 ) ) ;
#8816 = CARTESIAN_POINT ( 'NONE',  ( 1.653273178848927064E-15, 3.999999997815050889, -27.00000000000000355 ) ) ;
#8817 = EDGE_CURVE ( 'NONE', #369, #2588, #7279, .T. ) ;
#8818 = LINE ( 'NONE', #7290, #2402 ) ;
#8819 = CARTESIAN_POINT ( 'NONE',  ( -1.128215178125000273, -3.478124999385482141, -1.954126010382871259 ) ) ;
#8820 = CARTESIAN_POINT ( 'NONE',  ( -16.36254897777739004, 100.0000000000000142, 15.39785597259249350 ) ) ;
#8821 = CARTESIAN_POINT ( 'NONE',  ( -16.91946509138130139, 99.50000000000001421, 15.98858002463268413 ) ) ;
#8822 = CARTESIAN_POINT ( 'NONE',  ( 8.102924533678123709, 100.0000000000000000, 20.98904009517733726 ) ) ;
#8823 = ORIENTED_EDGE ( 'NONE', *, *, #3786, .F. ) ;
#8824 = AXIS2_PLACEMENT_3D ( 'NONE', #10037, #6790, #6953 ) ;
#8825 = CARTESIAN_POINT ( 'NONE',  ( 1.249999999999999334, -1.443749998770965881, -2.165063509461096825 ) ) ;
#8826 = ORIENTED_EDGE ( 'NONE', *, *, #3716, .T. ) ;
#8827 = DIRECTION ( 'NONE',  ( -0.9198211419112228837, 0.000000000000000000, 0.3923379498508065000 ) ) ;
#8828 = DIRECTION ( 'NONE',  ( 0.000000000000000000, -1.000000000000000000, 0.000000000000000000 ) ) ;
#8829 = ADVANCED_FACE ( 'NONE', ( #10108 ), #6854, .T. ) ;
#8830 = CARTESIAN_POINT ( 'NONE',  ( -14.75894607058735630, 100.0000000000000284, 15.77473972644577849 ) ) ;
#8831 = CARTESIAN_POINT ( 'NONE',  ( -1.128215178124998497, -4.115624999385482319, 1.954126010382872147 ) ) ;
#8832 = LINE ( 'NONE', #1505, #9115 ) ;
#8833 = AXIS2_PLACEMENT_3D ( 'NONE', #1979, #5768, #5173 ) ;
#8834 = SURFACE_STYLE_USAGE ( .BOTH. , #9618 ) ;
#8835 = CARTESIAN_POINT ( 'NONE',  ( 22.50000000000000355, 2.755455298081545172E-15, 0.000000000000000000 ) ) ;
#8836 = EDGE_CURVE ( 'NONE', #8637, #1444, #575, .T. ) ;
#8837 = CARTESIAN_POINT ( 'NONE',  ( 19.09188309203678813, 3.099999997815050090, -19.09188309203678813 ) ) ;
#8838 = CARTESIAN_POINT ( 'NONE',  ( 9.044794778432494908, 100.0000000000000142, 19.94873160813952140 ) ) ;
#8839 = ORIENTED_EDGE ( 'NONE', *, *, #191, .T. ) ;
#8840 = EDGE_CURVE ( 'NONE', #7555, #486, #274, .T. ) ;
#8841 = VECTOR ( 'NONE', #5091, 1000.000000000000114 ) ;
#8842 = CARTESIAN_POINT ( 'NONE',  ( -3.000000000000000888, -15.00000000000000000, 1.732050807568878303 ) ) ;
#8843 = CARTESIAN_POINT ( 'NONE',  ( 1.653273178848927064E-15, 4.799999997815051600, -27.00000000000000355 ) ) ;
#8844 = CARTESIAN_POINT ( 'NONE',  ( -2.256430356250000102, -4.753124999385482496, 0.000000000000000000 ) ) ;
#8845 = CARTESIAN_POINT ( 'NONE',  ( -21.16695614262292580, 99.50000000000000000, -11.33496398805607441 ) ) ;
#8846 = CARTESIAN_POINT ( 'NONE',  ( 11.36312591709336139, 4.499999998907525445, -27.43301270000000258 ) ) ;
#8847 = UNCERTAINTY_MEASURE_WITH_UNIT (LENGTH_MEASURE( 1.000000000000000082E-05 ), #8490, 'distance_accuracy_value', 'NONE');
#8848 = CARTESIAN_POINT ( 'NONE',  ( -20.66709314808276332, 100.0000000000000284, -10.01107456535036455 ) ) ;
#8849 = CARTESIAN_POINT ( 'NONE',  ( -7.500000000000000000, 104.5000000000000142, -0.9999999999999997780 ) ) ;
#8850 = CARTESIAN_POINT ( 'NONE',  ( 3.198738776810544415, 100.0000000000000142, -22.02447230026614022 ) ) ;
#8851 = FACE_OUTER_BOUND ( 'NONE', #5407, .T. ) ;
#8852 = CARTESIAN_POINT ( 'NONE',  ( -2.256430356249998770, -3.253124999385482941, 1.302750673588581876 ) ) ;
#8853 = CARTESIAN_POINT ( 'NONE',  ( 9.802580223201115217, 99.99999999999997158, 21.25247094773282086 ) ) ;
#8854 = ORIENTED_EDGE ( 'NONE', *, *, #7088, .T. ) ;
#8855 = CARTESIAN_POINT ( 'NONE',  ( -2.500000000000000000, -0.03749999999999999167, -1.443375672974064106 ) ) ;
#8856 = CARTESIAN_POINT ( 'NONE',  ( 27.43301269999999548, 1.899999998907525356, 11.36312591709337738 ) ) ;
#8857 = CARTESIAN_POINT ( 'NONE',  ( -15.72775836928289017, 99.50000000000000000, 17.03252426573849476 ) ) ;
#8858 = CARTESIAN_POINT ( 'NONE',  ( -19.09188309203678813, 3.700000000000000178, 19.09188309203678457 ) ) ;
#8859 = CYLINDRICAL_SURFACE ( 'NONE', #9212, 27.00000000000000355 ) ;
#8860 = ORIENTED_EDGE ( 'NONE', *, *, #5311, .F. ) ;
#8861 = FILL_AREA_STYLE ('',( #2373 ) ) ;
#8862 = DIRECTION ( 'NONE',  ( 0.9985355274883277454, 0.000000000000000000, -0.05409991075415104128 ) ) ;
#8863 =( BOUNDED_CURVE ( )  B_SPLINE_CURVE ( 2, ( #2710, #404, #5106, #6732, #2764, #8466, #2867, #6050, #9240 ),
 .UNSPECIFIED., .F., .F. ) 
 B_SPLINE_CURVE_WITH_KNOTS ( ( 3, 2, 2, 2, 3 ),
 ( 0.06250000000000000000, 0.06944444444444444753, 0.08333333333333332871, 0.09722222222222222376, 0.1041666666666666713 ),
 .UNSPECIFIED. ) 
 CURVE ( )  GEOMETRIC_REPRESENTATION_ITEM ( )  RATIONAL_B_SPLINE_CURVE ( ( 0.9330127018922194093, 0.9330127018922194093, 1.000000000000000000, 0.8660254037844387076, 1.000000000000000000, 0.8660254037844387076, 1.000000000000000000, 0.9330127018922192983, 0.9330127018922194093 ) ) 
 REPRESENTATION_ITEM ( '' )  );
#8864 = CARTESIAN_POINT ( 'NONE',  ( -20.72805389903318130, 99.99999999999994316, -9.848585782927868237 ) ) ;
#8865 = CARTESIAN_POINT ( 'NONE',  ( 27.43301270000000258, 2.649999998907525356, 0.000000000000000000 ) ) ;
#8866 = CARTESIAN_POINT ( 'NONE',  ( -11.18376618407358336, 2.149999999999999911, 26.99999999999999645 ) ) ;
#8867 = PRODUCT_DEFINITION_SHAPE ( 'NONE', 'NONE',  #8713 ) ;
#8868 = CARTESIAN_POINT ( 'NONE',  ( -22.33589105551819642, 100.0000000000000284, -11.18147695539509812 ) ) ;
#8869 = CARTESIAN_POINT ( 'NONE',  ( 1.128215178125001161, -2.803124999385482319, 1.954126010382870815 ) ) ;
#8870 = DIRECTION ( 'NONE',  ( -0.000000000000000000, -1.000000000000000000, -0.000000000000000000 ) ) ;
#8871 = CARTESIAN_POINT ( 'NONE',  ( 19.09188309203678102, 1.500000000000000000, 19.09188309203678813 ) ) ;
#8872 = CARTESIAN_POINT ( 'NONE',  ( 4.996790860652426159E-15, -1.912499999999999867, -2.500000000000000000 ) ) ;
#8873 = EDGE_CURVE ( 'NONE', #1383, #3372, #6637, .T. ) ;
#8874 = EDGE_CURVE ( 'NONE', #2013, #1313, #7502, .T. ) ;
#8875 = CARTESIAN_POINT ( 'NONE',  ( 2.500000000000000444, -3.806249998770965703, 1.443375672974063439 ) ) ;
#8876 = EDGE_LOOP ( 'NONE', ( #9046, #6947, #2216, #3794 ) ) ;
#8877 =( GEOMETRIC_REPRESENTATION_CONTEXT ( 3 ) GLOBAL_UNCERTAINTY_ASSIGNED_CONTEXT ( ( #9483 ) ) GLOBAL_UNIT_ASSIGNED_CONTEXT ( ( #10146, #1963, #2451 ) ) REPRESENTATION_CONTEXT ( 'NONE', 'WORKASPACE' ) );
#8878 = CARTESIAN_POINT ( 'NONE',  ( 4.570993444255353921, 99.99999999999998579, -21.37574484917381668 ) ) ;
#8879 = CARTESIAN_POINT ( 'NONE',  ( -10.49999999999999822, 104.5000000000000142, 0.000000000000000000 ) ) ;
#8880 = CARTESIAN_POINT ( 'NONE',  ( 9.820792995160308791, 99.50000000000000000, 20.21220011423140761 ) ) ;
#8881 = CARTESIAN_POINT ( 'NONE',  ( -2.256430356250000102, -4.228124999385483029, -1.302750673588580321 ) ) ;
#8882 = ADVANCED_FACE ( 'NONE', ( #4451 ), #6693, .T. ) ;
#8883 = CARTESIAN_POINT ( 'NONE',  ( 8.102924533678123709, 99.50000000000000000, 20.98904009517733726 ) ) ;
#8884 = DIRECTION ( 'NONE',  ( 0.000000000000000000, -1.000000000000000000, 0.000000000000000000 ) ) ;
#8885 = CARTESIAN_POINT ( 'NONE',  ( -14.83363727892122519, 99.50000000000001421, 15.50654517199034466 ) ) ;
#8886 = ORIENTED_EDGE ( 'NONE', *, *, #2860, .T. ) ;
#8887 = EDGE_CURVE ( 'NONE', #2926, #3621, #6992, .T. ) ;
#8888 = DIRECTION ( 'NONE',  ( -0.000000000000000000, -1.000000000000000000, -0.000000000000000000 ) ) ;
#8889 = CARTESIAN_POINT ( 'NONE',  ( 2.847408871211157155, 99.99999999999998579, -22.10537533382872510 ) ) ;
#8890 = CARTESIAN_POINT ( 'NONE',  ( -1.128215178125000273, -0.2156249993854829905, -1.954126010382871259 ) ) ;
#8891 = EDGE_CURVE ( 'NONE', #6656, #1438, #6749, .T. ) ;
#8892 = ORIENTED_EDGE ( 'NONE', *, *, #7878, .F. ) ;
#8893 = DIRECTION ( 'NONE',  ( 0.000000000000000000, 0.000000000000000000, -1.000000000000000000 ) ) ;
#8894 = CARTESIAN_POINT ( 'NONE',  ( 27.43301270000000258, 4.399999998907525800, -11.36312591709336139 ) ) ;
#8895 = CARTESIAN_POINT ( 'NONE',  ( -19.75840245672548789, 100.0000000000000000, -8.735905494466331689 ) ) ;
#8896 = DIRECTION ( 'NONE',  ( -0.7071067811865474617, -0.000000000000000000, 0.7071067811865476838 ) ) ;
#8897 = CARTESIAN_POINT ( 'NONE',  ( -16.35834224700816009, 99.50000000000000000, 16.43761959438736397 ) ) ;
#8898 = AXIS2_PLACEMENT_3D ( 'NONE', #9963, #4416, #283 ) ;
#8899 = CARTESIAN_POINT ( 'NONE',  ( -22.24883010645271852, 99.49999999999997158, -10.75389422444101939 ) ) ;
#8900 = CARTESIAN_POINT ( 'NONE',  ( 1.128215178124999607, -4.790624999385483029, -1.954126010382871259 ) ) ;
#8901 = ADVANCED_FACE ( 'NONE', ( #9947 ), #3935, .T. ) ;
#8902 = VERTEX_POINT ( 'NONE', #587 ) ;
#8903 = CARTESIAN_POINT ( 'NONE',  ( -1.128215178124998497, -5.015624999385482674, 1.954126010382872147 ) ) ;
#8904 = CYLINDRICAL_SURFACE ( 'NONE', #407, 2.500000000000000000 ) ;
#8905 = CARTESIAN_POINT ( 'NONE',  ( -27.00000000000000355, 4.400000000000000355, -3.306546357697854128E-15 ) ) ;
#8906 = CARTESIAN_POINT ( 'NONE',  ( 2.874264611687397331, 100.0000000000000142, -22.24889838548798693 ) ) ;
#8907 = EDGE_CURVE ( 'NONE', #6136, #3561, #3053, .T. ) ;
#8908 = DIRECTION ( 'NONE',  ( 0.000000000000000000, 0.000000000000000000, -1.000000000000000000 ) ) ;
#8909 = CARTESIAN_POINT ( 'NONE',  ( -20.89948324804827706, 99.50000000000001421, -10.26098411820691858 ) ) ;
#8910 = VERTEX_POINT ( 'NONE', #690 ) ;
#8911 = VERTEX_POINT ( 'NONE', #3882 ) ;
#8912 = AXIS2_PLACEMENT_3D ( 'NONE', #2149, #741, #3934 ) ;
#8913 = CARTESIAN_POINT ( 'NONE',  ( 3.472565890032746960, 100.0000000000000284, -24.54662015932514052 ) ) ;
#8914 = AXIS2_PLACEMENT_3D ( 'NONE', #10021, #6096, #4369 ) ;
#8915 = CARTESIAN_POINT ( 'NONE',  ( 0.000000000000000000, 97.00000000000000000, -24.00000000000000355 ) ) ;
#8916 = DIRECTION ( 'NONE',  ( 1.000000000000000000, 0.000000000000000000, 0.000000000000000000 ) ) ;
#8917 = CARTESIAN_POINT ( 'NONE',  ( -2.256430356250000102, -3.890624999385481786, -1.302750673588580321 ) ) ;
#8918 = CARTESIAN_POINT ( 'NONE',  ( -27.00000000000001421, 1.849999997815050534, 11.18376618407356560 ) ) ;
#8919 = CARTESIAN_POINT ( 'NONE',  ( -16.92301558088953328, 100.0000000000000142, 15.88693424423437683 ) ) ;
#8920 = CARTESIAN_POINT ( 'NONE',  ( 3.739209042966563867, 99.50000000000000000, -21.42288334414699236 ) ) ;
#8921 =( GEOMETRIC_REPRESENTATION_CONTEXT ( 3 ) GLOBAL_UNCERTAINTY_ASSIGNED_CONTEXT ( ( #8847 ) ) GLOBAL_UNIT_ASSIGNED_CONTEXT ( ( #8490, #1370, #4620 ) ) REPRESENTATION_CONTEXT ( 'NONE', 'WORKASPACE' ) );
#8922 =( BOUNDED_CURVE ( )  B_SPLINE_CURVE ( 1, ( #8956, #6640 ),
 .UNSPECIFIED., .F., .T. ) 
 B_SPLINE_CURVE_WITH_KNOTS ( ( 2, 2 ),
 ( 0.000000000000000000, 1.000000000000000000 ),
 .UNSPECIFIED. ) 
 CURVE ( )  GEOMETRIC_REPRESENTATION_ITEM ( )  RATIONAL_B_SPLINE_CURVE ( ( 0.9401542295229976531, 0.9401542295229976531 ) ) 
 REPRESENTATION_ITEM ( '' )  );
#8923 = CARTESIAN_POINT ( 'NONE',  ( 5.302876193624534821E-16, -4.781249998770966236, 2.886751345948128655 ) ) ;
#8924 = ORIENTED_EDGE ( 'NONE', *, *, #4672, .F. ) ;
#8925 = CARTESIAN_POINT ( 'NONE',  ( 3.207057600658871355, 99.50000000000000000, -22.07913334414698880 ) ) ;
#8926 = FACE_OUTER_BOUND ( 'NONE', #9903, .T. ) ;
#8927 = CARTESIAN_POINT ( 'NONE',  ( -22.28244091826395135, 99.50000000000000000, -10.68852969318427881 ) ) ;
#8928 = CARTESIAN_POINT ( 'NONE',  ( -2.256430356250000102, -4.678124999385483207, -1.302750673588580321 ) ) ;
#8929 = EDGE_LOOP ( 'NONE', ( #7257, #6770, #8948, #9224, #6540 ) ) ;
#8930 = DIRECTION ( 'NONE',  ( 0.000000000000000000, 0.000000000000000000, 1.000000000000000000 ) ) ;
#8931 = DIRECTION ( 'NONE',  ( -0.000000000000000000, 1.000000000000000000, -0.000000000000000000 ) ) ;
#8932 = CARTESIAN_POINT ( 'NONE',  ( 2.500000000000000444, -3.806249998770965703, 1.443375672974063439 ) ) ;
#8933 = ORIENTED_EDGE ( 'NONE', *, *, #4474, .T. ) ;
#8934 = B_SPLINE_CURVE_WITH_KNOTS ( 'NONE', 3,
 ( #6255, #3900, #6925, #10125, #8616, #7713, #2226, #3743, #4688, #9341, #8445, #5428, #3687, #6310, #657, #2171, #1441, #5369, #2904 ),
 .UNSPECIFIED., .F., .F.,
 ( 4, 1, 1, 1, 1, 1, 1, 1, 1, 1, 1, 1, 1, 1, 1, 1, 4 ),
 ( 0.000000000000000000, 0.06505403082392276215, 0.1283503816230405770, 0.1902281050068566903, 0.2509397092642763338, 0.3119571365542418429, 0.3738829716944830350, 0.4367040802691206092, 0.5009896104483916313, 0.5655726868558689224, 0.6286067690057803858, 0.6898677555008378981, 0.7506620835893632604, 0.8110632348575060879, 0.8726242918051292374, 0.9355756365154705989, 0.9999999999999998890 ),
 .UNSPECIFIED. ) ;
#8935 = FACE_OUTER_BOUND ( 'NONE', #2007, .T. ) ;
#8936 = VECTOR ( 'NONE', #7180, 1000.000000000000000 ) ;
#8937 = EDGE_CURVE ( 'NONE', #3431, #3123, #8752, .T. ) ;
#8938 = CARTESIAN_POINT ( 'NONE',  ( 3.238942592553923472, 99.50000000000001421, -24.36085717291697250 ) ) ;
#8939 = FACE_OUTER_BOUND ( 'NONE', #8093, .T. ) ;
#8940 = CARTESIAN_POINT ( 'NONE',  ( 2.874264611687397331, 99.50000000000001421, -22.24889838548798693 ) ) ;
#8941 = CARTESIAN_POINT ( 'NONE',  ( -27.00000000000000355, 3.399999997815049912, -3.306546357697854128E-15 ) ) ;
#8942 = CARTESIAN_POINT ( 'NONE',  ( 2.940631318607589417, 100.0000000000000000, -23.77584808773673331 ) ) ;
#8943 = DIRECTION ( 'NONE',  ( -0.000000000000000000, -1.000000000000000000, -0.000000000000000000 ) ) ;
#8944 = CARTESIAN_POINT ( 'NONE',  ( 3.204253864046738176, 100.0000000000000000, -22.06071064728738662 ) ) ;
#8945 = CARTESIAN_POINT ( 'NONE',  ( -21.99951964646687941, 99.50000000000001421, -11.00094659099690553 ) ) ;
#8946 = CARTESIAN_POINT ( 'NONE',  ( -1.128215178124998497, -5.015624999385482674, 1.954126010382872147 ) ) ;
#8947 = AXIS2_PLACEMENT_3D ( 'NONE', #6485, #3929, #9531 ) ;
#8948 = ORIENTED_EDGE ( 'NONE', *, *, #3337, .T. ) ;
#8949 = CARTESIAN_POINT ( 'NONE',  ( -2.256430356250000102, -3.778124999385482408, -1.302750673588580321 ) ) ;
#8950 =( NAMED_UNIT ( * ) SI_UNIT ( $, .STERADIAN. ) SOLID_ANGLE_UNIT ( ) );
#8951 = CARTESIAN_POINT ( 'NONE',  ( -15.03933290382598820, 99.50000000000000000, 15.19633946010233849 ) ) ;
#8952 = VECTOR ( 'NONE', #5057, 999.9999999999998863 ) ;
#8953 = CARTESIAN_POINT ( 'NONE',  ( 2.936358689207804851, 99.50000000000000000, -23.74786164940363875 ) ) ;
#8954 = CARTESIAN_POINT ( 'NONE',  ( 19.09188309203678813, 4.899999999999999467, -19.09188309203678813 ) ) ;
#8955 = LINE ( 'NONE', #1772, #4055 ) ;
#8956 = CARTESIAN_POINT ( 'NONE',  ( -1.728530063377412107, -5.141148402510967053, -1.450400555903694988 ) ) ;
#8957 = CARTESIAN_POINT ( 'NONE',  ( 4.232798786556307036, 100.0000000000000000, -24.34936571594186105 ) ) ;
#8958 = CARTESIAN_POINT ( 'NONE',  ( -4.959819536546781389E-15, 1.999999997815050445, 27.00000000000000355 ) ) ;
#8959 = CIRCLE ( 'NONE', #5940, 18.00000000000000000 ) ;
#8960 = VERTEX_POINT ( 'NONE', #744 ) ;
#8961 = CARTESIAN_POINT ( 'NONE',  ( 7.726884419709978857, 99.50000000000000000, 20.74516479202295471 ) ) ;
#8962 = EDGE_CURVE ( 'NONE', #9616, #9118, #667, .T. ) ;
#8963 = CARTESIAN_POINT ( 'NONE',  ( 2.500000000000000000, -1.518749998770965837, -3.061616997868383141E-16 ) ) ;
#8964 = CARTESIAN_POINT ( 'NONE',  ( -16.25072943800822500, 99.50000000000005684, 15.30228603765648820 ) ) ;
#8965 = EDGE_CURVE ( 'NONE', #9210, #2398, #5658, .T. ) ;
#8966 = CARTESIAN_POINT ( 'NONE',  ( -21.29537297865864431, 99.50000000000000000, -11.39144590536739976 ) ) ;
#8967 = CARTESIAN_POINT ( 'NONE',  ( 1.128215178125001161, -3.703124999385482230, 1.954126010382870815 ) ) ;
#8968 = CARTESIAN_POINT ( 'NONE',  ( 9.044794778432494908, 99.50000000000001421, 19.94873160813952140 ) ) ;
#8969 = CARTESIAN_POINT ( 'NONE',  ( -16.79604063091391097, 99.50000000000000000, 15.40463673182947701 ) ) ;
#8970 = VECTOR ( 'NONE', #9563, 1000.000000000000000 ) ;
#8971 = CARTESIAN_POINT ( 'NONE',  ( 4.401614252286283779, 100.0000000000000284, -24.65974366035752396 ) ) ;
#8972 = CARTESIAN_POINT ( 'NONE',  ( -2.256430356250000102, -0.2531249993854829405, 0.000000000000000000 ) ) ;
#8973 = ORIENTED_EDGE ( 'NONE', *, *, #3496, .T. ) ;
#8974 = VECTOR ( 'NONE', #8292, 1000.000000000000000 ) ;
#8975 = CARTESIAN_POINT ( 'NONE',  ( -22.33589105551819642, 100.0000000000000284, -11.18147695539509812 ) ) ;
#8976 = DIRECTION ( 'NONE',  ( 0.000000000000000000, -1.000000000000000000, 0.000000000000000000 ) ) ;
#8977 = DIRECTION ( 'NONE',  ( 0.08704561088320925122, 0.9949358851208914833, -0.05025580687519624196 ) ) ;
#8978 = CARTESIAN_POINT ( 'NONE',  ( 4.688812652749139609, 99.50000000000001421, -24.54863390154074310 ) ) ;
#8979 = ORIENTED_EDGE ( 'NONE', *, *, #7162, .T. ) ;
#8980 = DIRECTION ( 'NONE',  ( -0.000000000000000000, 1.000000000000000000, -0.000000000000000000 ) ) ;
#8981 = DIRECTION ( 'NONE',  ( 0.000000000000000000, 0.000000000000000000, -1.000000000000000000 ) ) ;
#8982 = CARTESIAN_POINT ( 'NONE',  ( -21.58460863908062066, 100.0000000000000284, -11.10356610083683648 ) ) ;
#8983 = ORIENTED_EDGE ( 'NONE', *, *, #2927, .T. ) ;
#8984 = CARTESIAN_POINT ( 'NONE',  ( 4.187832255138415505, 99.50000000000001421, -21.50835573230103037 ) ) ;
#8985 = AXIS2_PLACEMENT_3D ( 'NONE', #1964, #8357, #1085 ) ;
#8986 = CARTESIAN_POINT ( 'NONE',  ( 4.122675185292913547, 99.99999999999994316, -22.83451320417363561 ) ) ;
#8987 = CARTESIAN_POINT ( 'NONE',  ( 7.734522023158566739, 99.99999999999997158, 20.86022014488863618 ) ) ;
#8988 = LINE ( 'NONE', #8253, #8439 ) ;
#8989 = CARTESIAN_POINT ( 'NONE',  ( 11.18376618407356915, 3.949999997815050179, -27.00000000000000355 ) ) ;
#8990 = CARTESIAN_POINT ( 'NONE',  ( 10.85214315541671759, 99.50000000000000000, 22.51047735782115211 ) ) ;
#8991 = CARTESIAN_POINT ( 'NONE',  ( -21.00001322343447541, 100.0000000000000142, -9.990026185521596602 ) ) ;
#8992 = CARTESIAN_POINT ( 'NONE',  ( -15.32348647777738826, 100.0000000000000000, 15.39505148541300450 ) ) ;
#8993 = EDGE_CURVE ( 'NONE', #7561, #9475, #4123, .T. ) ;
#8994 = CARTESIAN_POINT ( 'NONE',  ( -22.20893716642541804, 100.0000000000000284, -10.81429252070940272 ) ) ;
#8995 = CARTESIAN_POINT ( 'NONE',  ( 3.023131990384279710, 100.0000000000000284, -21.47496011329876708 ) ) ;
#8996 = CARTESIAN_POINT ( 'NONE',  ( -3.486133158594716510E-16, -2.362499999999999378, -2.500000000000000000 ) ) ;
#8997 = ORIENTED_EDGE ( 'NONE', *, *, #7717, .F. ) ;
#8998 = CARTESIAN_POINT ( 'NONE',  ( -1.250000000000000222, -0.07499999999999999722, -2.165063509461096825 ) ) ;
#8999 =( NAMED_UNIT ( * ) PLANE_ANGLE_UNIT ( ) SI_UNIT ( $, .RADIAN. ) );
#9000 = CARTESIAN_POINT ( 'NONE',  ( -0.6698729810778020211, -2.792403810567666067, -2.500000000000002665 ) ) ;
#9001 = CARTESIAN_POINT ( 'NONE',  ( 2.940631318607589417, 99.50000000000000000, -23.77584808773673331 ) ) ;
#9002 = CARTESIAN_POINT ( 'NONE',  ( 11.36312591709336850, 4.099999998907525089, 27.43301269999999903 ) ) ;
#9003 = CARTESIAN_POINT ( 'NONE',  ( -27.00000000000000355, 0.4000000000000000222, -3.306546357697854128E-15 ) ) ;
#9004 = DIRECTION ( 'NONE',  ( 0.000000000000000000, 1.000000000000000000, 0.000000000000000000 ) ) ;
#9005 = CARTESIAN_POINT ( 'NONE',  ( -21.12798922145720582, 99.99999999999998579, -10.90888695829967325 ) ) ;
#9006 = EDGE_CURVE ( 'NONE', #4720, #3772, #2747, .T. ) ;
#9007 = ORIENTED_EDGE ( 'NONE', *, *, #4397, .F. ) ;
#9008 = CARTESIAN_POINT ( 'NONE',  ( -22.08823018108446234, 99.50000000000000000, -9.406177930363766038 ) ) ;
#9009 = CARTESIAN_POINT ( 'NONE',  ( 2.971063225226878046, 100.0000000000000000, -23.91837856253154015 ) ) ;
#9010 = LINE ( 'NONE', #4247, #4881 ) ;
#9011 = DIRECTION ( 'NONE',  ( 0.000000000000000000, 0.000000000000000000, 1.000000000000000000 ) ) ;
#9012 = CARTESIAN_POINT ( 'NONE',  ( -16.49882833452567965, 99.99999999999995737, 15.05677840364783115 ) ) ;
#9013 = CARTESIAN_POINT ( 'NONE',  ( 9.245739950628269810, 99.50000000000002842, 20.03726560014620617 ) ) ;
#9014 = LINE ( 'NONE', #6025, #7103 ) ;
#9015 = CARTESIAN_POINT ( 'NONE',  ( 19.09188309203678102, 2.299999999999999822, 19.09188309203678813 ) ) ;
#9016 = ADVANCED_FACE ( 'NONE', ( #5664 ), #898, .T. ) ;
#9017 = B_SPLINE_CURVE_WITH_KNOTS ( 'NONE', 3,
 ( #6206, #6038, #9286, #3747, #9179, #7777, #9228, #9404, #9969, #6151, #6821, #2060, #4421, #1999, #5198, #9348, #8396, #5254, #442 ),
 .UNSPECIFIED., .F., .F.,
 ( 4, 1, 1, 1, 1, 1, 1, 1, 1, 1, 1, 1, 1, 1, 1, 1, 4 ),
 ( 0.000000000000000000, 0.06363772181477481138, 0.1253661190162797812, 0.1854850957718461035, 0.2454326483351531030, 0.3054881917026986415, 0.3659564384638642753, 0.4275766838088623234, 0.4913505196498278993, 0.5556437034595619329, 0.6183735394983103095, 0.6802114403575724166, 0.7422401234104337719, 0.8041288543812358247, 0.8678488776753463529, 0.9326351893241184854, 1.000000000000000000 ),
 .UNSPECIFIED. ) ;
#9018 = EDGE_CURVE ( 'NONE', #6706, #1490, #4653, .T. ) ;
#9019 = CARTESIAN_POINT ( 'NONE',  ( 5.302876193624534821E-16, -3.431249998770965259, 2.886751345948128655 ) ) ;
#9020 = ORIENTED_EDGE ( 'NONE', *, *, #10119, .F. ) ;
#9021 = VERTEX_POINT ( 'NONE', #7447 ) ;
#9022 = CARTESIAN_POINT ( 'NONE',  ( -21.71039561923405969, 100.0000000000000426, -11.44438725057713313 ) ) ;
#9023 = CARTESIAN_POINT ( 'NONE',  ( 3.356341388373609291, 99.50000000000001421, -21.61643044175963979 ) ) ;
#9024 = CARTESIAN_POINT ( 'NONE',  ( 4.154273145530666511, 99.50000000000000000, -22.82723029927519676 ) ) ;
#9025 = CARTESIAN_POINT ( 'NONE',  ( -15.15871127190382417, 100.0000000000000000, 15.63231653451427761 ) ) ;
#9026 = PLANE ( 'NONE',  #7624 ) ;
#9027 = EDGE_CURVE ( 'NONE', #7011, #9169, #1767, .T. ) ;
#9028 = COLOUR_RGB ( '',0.8941176470588234615, 0.8941176470588234615, 0.8941176470588234615 ) ;
#9029 = LINE ( 'NONE', #1846, #9338 ) ;
#9030 = DIRECTION ( 'NONE',  ( -0.000000000000000000, -0.000000000000000000, -1.000000000000000000 ) ) ;
#9031 = ORIENTED_EDGE ( 'NONE', *, *, #2850, .F. ) ;
#9032 = FACE_OUTER_BOUND ( 'NONE', #9525, .T. ) ;
#9033 = CARTESIAN_POINT ( 'NONE',  ( 19.39806930854668110, 5.149999998907524912, -19.39806930854668110 ) ) ;
#9034 = LINE ( 'NONE', #3647, #8573 ) ;
#9035 = B_SPLINE_CURVE_WITH_KNOTS ( 'NONE', 3,
 ( #4029, #936, #8742, #45, #10266, #5653, #7954, #1566, #4811, #9625, #8694, #3098, #4756, #787, #3979 ),
 .UNSPECIFIED., .F., .F.,
 ( 4, 1, 1, 1, 1, 1, 1, 1, 1, 1, 1, 1, 4 ),
 ( 0.000000000000000000, 0.1055296353700490852, 0.2070742529895955586, 0.3056622059958778448, 0.4023599870273183998, 0.4943057198019382148, 0.5778637904027289496, 0.6550095244395398586, 0.7278863574113029200, 0.7976678238154090161, 0.8645871040366396310, 0.9319858836656568224, 1.000000000000000000 ),
 .UNSPECIFIED. ) ;
#9036 = CARTESIAN_POINT ( 'NONE',  ( 24.00000000000000711, 71.18660744634364335, -2.939152317953649078E-15 ) ) ;
#9037 = CARTESIAN_POINT ( 'NONE',  ( 4.049441352997683374, 99.99999999999997158, -21.43849541167161732 ) ) ;
#9038 = CARTESIAN_POINT ( 'NONE',  ( -15.31787750341841559, 100.0000000000000000, 16.43551622900274722 ) ) ;
#9039 = CARTESIAN_POINT ( 'NONE',  ( -27.00000000000000355, 2.599999997815050534, -3.306546357697854128E-15 ) ) ;
#9040 = LINE ( 'NONE', #9871, #3946 ) ;
#9041 = CARTESIAN_POINT ( 'NONE',  ( -21.45221949983897858, 100.0000000000000000, -9.661157428473494235 ) ) ;
#9042 = CARTESIAN_POINT ( 'NONE',  ( 3.293841816516395848, 99.99999999999998579, -23.44781013845121009 ) ) ;
#9043 = CARTESIAN_POINT ( 'NONE',  ( -22.24883010645271852, 99.99999999999997158, -10.75389422444101939 ) ) ;
#9044 = DIRECTION ( 'NONE',  ( -0.9567912676219745283, 0.000000000000000000, 0.2907756355032780071 ) ) ;
#9045 = CARTESIAN_POINT ( 'NONE',  ( 0.000000000000000000, 100.0000000000000000, -27.00000000000000355 ) ) ;
#9046 = ORIENTED_EDGE ( 'NONE', *, *, #956, .F. ) ;
#9047 = CARTESIAN_POINT ( 'NONE',  ( 2.256430356249999658, -4.378124999385482496, -1.302750673588581432 ) ) ;
#9048 = EDGE_CURVE ( 'NONE', #7160, #4075, #394, .T. ) ;
#9049 = CARTESIAN_POINT ( 'NONE',  ( -15.56505537928961047, 99.50000000000002842, 14.87309967080592088 ) ) ;
#9050 = CARTESIAN_POINT ( 'NONE',  ( 2.852289972453743161, 99.50000000000000000, -22.14293542748032451 ) ) ;
#9051 = EDGE_CURVE ( 'NONE', #4536, #1968, #1172, .T. ) ;
#9052 = B_SPLINE_CURVE_WITH_KNOTS ( 'NONE', 3,
 ( #3539, #5843, #8940, #401, #4226, #7509, #9818, #1758, #347, #1856, #6728 ),
 .UNSPECIFIED., .F., .F.,
 ( 4, 1, 1, 1, 1, 1, 1, 1, 4 ),
 ( 0.000000000000000000, 0.1243175037779491315, 0.2437391319546453605, 0.3610119291759345539, 0.4796059399169178006, 0.5994854737745749507, 0.7252340722053824962, 0.8585022233306516259, 1.000000000000000000 ),
 .UNSPECIFIED. ) ;
#9053 = CARTESIAN_POINT ( 'NONE',  ( -19.39806930854668465, 3.949999998907525178, 19.39806930854667755 ) ) ;
#9054 = CARTESIAN_POINT ( 'NONE',  ( -0.6698729810778054627, -0.8075961894323341328, 2.500000000000000000 ) ) ;
#9055 = VECTOR ( 'NONE', #6315, 1000.000000000000114 ) ;
#9056 = DIRECTION ( 'NONE',  ( 0.000000000000000000, -1.000000000000000000, 0.000000000000000000 ) ) ;
#9057 = DIRECTION ( 'NONE',  ( 0.000000000000000000, 0.000000000000000000, 1.000000000000000000 ) ) ;
#9058 = CARTESIAN_POINT ( 'NONE',  ( -11.18376618407358336, 4.349999997815050534, 26.99999999999999645 ) ) ;
#9059 = EDGE_LOOP ( 'NONE', ( #4443, #6868, #2761, #7223 ) ) ;
#9060 = CARTESIAN_POINT ( 'NONE',  ( 7.753999887479250397, 99.50000000000000000, 20.97676509141502166 ) ) ;
#9061 = CARTESIAN_POINT ( 'NONE',  ( -27.43301270000000258, 4.599999998907525978, -11.36312591709336317 ) ) ;
#9062 = DIRECTION ( 'NONE',  ( 0.000000000000000000, 0.000000000000000000, -1.000000000000000000 ) ) ;
#9063 = CARTESIAN_POINT ( 'NONE',  ( -21.43094455402013310, 99.50000000000000000, -11.42705968398779426 ) ) ;
#9064 = CARTESIAN_POINT ( 'NONE',  ( 4.472992770554171216, 99.99999999999998579, -21.83386288566719458 ) ) ;
#9065 = CARTESIAN_POINT ( 'NONE',  ( -4.357666448243394824E-15, -2.531249998770965348, 2.500000000000000000 ) ) ;
#9066 = EDGE_CURVE ( 'NONE', #341, #2567, #9287, .T. ) ;
#9067 = CARTESIAN_POINT ( 'NONE',  ( 9.583828860305853681, 99.99999999999992895, 20.68614437522342797 ) ) ;
#9068 = DIRECTION ( 'NONE',  ( 1.000000000000000000, 0.000000000000000000, -0.000000000000000000 ) ) ;
#9069 =( BOUNDED_CURVE ( )  B_SPLINE_CURVE ( 2, ( #7231, #9547, #4728, #4148, #5723, #6454, #167, #6502, #3355 ),
 .UNSPECIFIED., .F., .T. ) 
 B_SPLINE_CURVE_WITH_KNOTS ( ( 3, 2, 2, 2, 3 ),
 ( 0.6041666666666667407, 0.6111111111111111605, 0.6250000000000000000, 0.6388888888888888395, 0.6458333333333333703 ),
 .UNSPECIFIED. ) 
 CURVE ( )  GEOMETRIC_REPRESENTATION_ITEM ( )  RATIONAL_B_SPLINE_CURVE ( ( 0.9330127018922192983, 0.9330127018922198534, 1.000000000000000000, 0.8660254037844387076, 1.000000000000000000, 0.8660254037844387076, 1.000000000000000000, 0.9330127018922187432, 0.9330127018922192983 ) ) 
 REPRESENTATION_ITEM ( '' )  );
#9070 = VERTEX_POINT ( 'NONE', #2178 ) ;
#9071 = CARTESIAN_POINT ( 'NONE',  ( -16.35834224700816009, 99.50000000000000000, 16.43761959438736397 ) ) ;
#9072 = PRESENTATION_LAYER_ASSIGNMENT (  '', '', ( #9415 ) ) ;
#9073 = CARTESIAN_POINT ( 'NONE',  ( 1.249999999999999334, -3.693749998770965437, -2.165063509461096825 ) ) ;
#9074 = VERTEX_POINT ( 'NONE', #502 ) ;
#9075 =( REPRESENTATION_RELATIONSHIP ('NONE','NONE', #3375, #2324 ) REPRESENTATION_RELATIONSHIP_WITH_TRANSFORMATION ( #44 )SHAPE_REPRESENTATION_RELATIONSHIP( ) );
#9076 = CARTESIAN_POINT ( 'NONE',  ( 3.681717055787076642, 100.0000000000000000, -21.09125273517263111 ) ) ;
#9077 = CARTESIAN_POINT ( 'NONE',  ( 3.552835461024879127, 99.50000000000000000, -21.47801279722421697 ) ) ;
#9078 = LINE ( 'NONE', #5194, #883 ) ;
#9079 = CARTESIAN_POINT ( 'NONE',  ( -15.13293277027690209, 100.0000000000000000, 16.13104881108577970 ) ) ;
#9080 = FACE_OUTER_BOUND ( 'NONE', #4506, .T. ) ;
#9081 = CARTESIAN_POINT ( 'NONE',  ( 4.739008722453744049, 100.0000000000000142, -24.06821587619827696 ) ) ;
#9082 = CARTESIAN_POINT ( 'NONE',  ( 3.597125852879613728, 99.49999999999998579, -24.22990373345680126 ) ) ;
#9083 = ORIENTED_EDGE ( 'NONE', *, *, #4088, .F. ) ;
#9084 = FACE_OUTER_BOUND ( 'NONE', #8467, .T. ) ;
#9085 = CARTESIAN_POINT ( 'NONE',  ( 19.39806930854667399, 4.249999998907525445, 19.39806930854668465 ) ) ;
#9086 = DIRECTION ( 'NONE',  ( 0.000000000000000000, 0.000000000000000000, 1.000000000000000000 ) ) ;
#9087 = EDGE_CURVE ( 'NONE', #498, #7819, #7044, .T. ) ;
#9088 = CARTESIAN_POINT ( 'NONE',  ( 21.47055288461538325, 99.50000000000000000, -0.7081330128205128860 ) ) ;
#9089 = CARTESIAN_POINT ( 'NONE',  ( 7.753999887479250397, 99.99999999999994316, 20.97676509141502166 ) ) ;
#9090 = ORIENTED_EDGE ( 'NONE', *, *, #8242, .F. ) ;
#9091 = CARTESIAN_POINT ( 'NONE',  ( 3.252389375388976323, 100.0000000000000711, -22.22144413113850447 ) ) ;
#9092 = CARTESIAN_POINT ( 'NONE',  ( -11.18376618407358336, 3.549999997815050268, 26.99999999999999645 ) ) ;
#9093 = DIRECTION ( 'NONE',  ( 0.000000000000000000, -1.000000000000000000, 0.000000000000000000 ) ) ;
#9094 = CARTESIAN_POINT ( 'NONE',  ( 2.143131898507868643E-15, 105.0000000000000142, 17.50000000000000355 ) ) ;
#9095 = CARTESIAN_POINT ( 'NONE',  ( 4.122675185292913547, 99.99999999999997158, -22.83451320417363561 ) ) ;
#9096 = CARTESIAN_POINT ( 'NONE',  ( -21.93524539549613550, 99.99999999999998579, -11.03420246938663318 ) ) ;
#9097 = DIRECTION ( 'NONE',  ( 0.000000000000000000, -1.000000000000000000, 0.000000000000000000 ) ) ;
#9098 = CARTESIAN_POINT ( 'NONE',  ( 4.786228327491940187E-16, -4.978124999385483029, 2.605501347177161087 ) ) ;
#9099 = CARTESIAN_POINT ( 'NONE',  ( -2.500000000000000000, -2.737499999999999822, -1.443375672974064106 ) ) ;
#9100 = CARTESIAN_POINT ( 'NONE',  ( -14.74935495356232984, 99.50000000000001421, 15.91322402822111926 ) ) ;
#9101 = CARTESIAN_POINT ( 'NONE',  ( -1.595409442497313560E-16, -0.3656249993854829294, -2.605501347177161087 ) ) ;
#9102 = CARTESIAN_POINT ( 'NONE',  ( 19.39806930854668110, 3.549999998907525267, -19.39806930854668110 ) ) ;
#9103 = CARTESIAN_POINT ( 'NONE',  ( -19.09188309203678813, 0.5000000000000000000, 19.09188309203678457 ) ) ;
#9104 = DIRECTION ( 'NONE',  ( -0.5137073458062109133, 0.000000000000000000, -0.8579654788304353907 ) ) ;
#9105 = FACE_OUTER_BOUND ( 'NONE', #7527, .T. ) ;
#9106 = CARTESIAN_POINT ( 'NONE',  ( 7.746148141271532950, 100.0000000000000284, 20.51930889200067298 ) ) ;
#9107 = CIRCLE ( 'NONE', #420, 25.15000000000000213 ) ;
#9108 = ORIENTED_EDGE ( 'NONE', *, *, #9605, .F. ) ;
#9109 = DIRECTION ( 'NONE',  ( 0.000000000000000000, 0.000000000000000000, -1.000000000000000000 ) ) ;
#9110 = DIRECTION ( 'NONE',  ( 0.04357787137382919396, -0.9961946980917455452, -0.07547908730517349785 ) ) ;
#9111 = PLANE ( 'NONE',  #4283 ) ;
#9112 = CARTESIAN_POINT ( 'NONE',  ( 9.554054106072296548, 99.50000000000001421, 20.45778517829714360 ) ) ;
#9113 = CARTESIAN_POINT ( 'NONE',  ( -21.16695614262292580, 99.50000000000000000, -11.33496398805607441 ) ) ;
#9114 = CARTESIAN_POINT ( 'NONE',  ( 4.786228327491940187E-16, -5.090624999385482852, 2.605501347177161087 ) ) ;
#9115 = VECTOR ( 'NONE', #879, 1000.000000000000227 ) ;
#9116 = CARTESIAN_POINT ( 'NONE',  ( 9.389534246205572643, 99.50000000000001421, 21.46805835725047729 ) ) ;
#9117 = CARTESIAN_POINT ( 'NONE',  ( 11.18376618407357626, 2.250000000000000888, 27.00000000000000000 ) ) ;
#9118 = VERTEX_POINT ( 'NONE', #10249 ) ;
#9119 = AXIS2_PLACEMENT_3D ( 'NONE', #6733, #9873, #2521 ) ;
#9120 = CARTESIAN_POINT ( 'NONE',  ( -16.34021191015031249, 99.50000000000000000, 16.45483272884350967 ) ) ;
#9121 = CARTESIAN_POINT ( 'NONE',  ( -2.256430356249999214, -2.915624999385482585, 1.302750673588581876 ) ) ;
#9122 = EDGE_LOOP ( 'NONE', ( #7885, #1727 ) ) ;
#9123 = EDGE_CURVE ( 'NONE', #9182, #8764, #954, .T. ) ;
#9124 = CARTESIAN_POINT ( 'NONE',  ( -22.51488550592518934, 99.49999999999997158, -10.97145172607810615 ) ) ;
#9125 = PLANE ( 'NONE',  #4634 ) ;
#9126 = CARTESIAN_POINT ( 'NONE',  ( -27.00000000000000355, 4.949999997815051067, -11.18376618407357270 ) ) ;
#9127 =( BOUNDED_CURVE ( )  B_SPLINE_CURVE ( 2, ( #2225, #10066, #1274, #7656, #1994, #6087, #5368, #2053, #3020 ),
 .UNSPECIFIED., .F., .F. ) 
 B_SPLINE_CURVE_WITH_KNOTS ( ( 3, 2, 2, 2, 3 ),
 ( 0.1041666666666666713, 0.1111111111111111049, 0.1250000000000000000, 0.1388888888888888951, 0.1458333333333333426 ),
 .UNSPECIFIED. ) 
 CURVE ( )  GEOMETRIC_REPRESENTATION_ITEM ( )  RATIONAL_B_SPLINE_CURVE ( ( 0.9330127018922194093, 0.9330127018922194093, 1.000000000000000000, 0.8660254037844387076, 1.000000000000000000, 0.8660254037844387076, 1.000000000000000000, 0.9330127018922194093, 0.9330127018922194093 ) ) 
 REPRESENTATION_ITEM ( '' )  );
#9128 = CARTESIAN_POINT ( 'NONE',  ( 4.599186066243659887, 99.50000000000002842, -24.59301055568561623 ) ) ;
#9129 = CARTESIAN_POINT ( 'NONE',  ( -15.10382517959271098, 99.49999999999998579, 15.91526905993627317 ) ) ;
#9130 = AXIS2_PLACEMENT_3D ( 'NONE', #5094, #2698, #340 ) ;
#9131 = CARTESIAN_POINT ( 'NONE',  ( -2.499999999999999556, -0.8062499987709659255, 1.443375672974065882 ) ) ;
#9132 = CARTESIAN_POINT ( 'NONE',  ( -21.99951964646687941, 100.0000000000000142, -11.00094659099690553 ) ) ;
#9133 = DIRECTION ( 'NONE',  ( 0.000000000000000000, 0.000000000000000000, 1.000000000000000000 ) ) ;
#9134 = ORIENTED_EDGE ( 'NONE', *, *, #7239, .F. ) ;
#9135 = CARTESIAN_POINT ( 'NONE',  ( 0.000000000000000000, 0.000000000000000000, 0.000000000000000000 ) ) ;
#9136 = CARTESIAN_POINT ( 'NONE',  ( 27.43301269999999548, 5.099999998907525978, 11.36312591709337738 ) ) ;
#9137 = CARTESIAN_POINT ( 'NONE',  ( -7.500000000000000000, 105.0000000000000142, -0.9999999999999997780 ) ) ;
#9138 = CARTESIAN_POINT ( 'NONE',  ( 3.472565890032746960, 99.50000000000002842, -24.54662015932514052 ) ) ;
#9139 = CARTESIAN_POINT ( 'NONE',  ( 3.775125937424839151, 99.50000000000000000, -21.41825520325024712 ) ) ;
#9140 = ORIENTED_EDGE ( 'NONE', *, *, #4805, .T. ) ;
#9141 = CARTESIAN_POINT ( 'NONE',  ( 3.563396934924631942, 100.0000000000000426, -22.47881610735839431 ) ) ;
#9142 = CARTESIAN_POINT ( 'NONE',  ( -27.00000000000000355, 3.349999997815050090, -11.18376618407357093 ) ) ;
#9143 = EDGE_CURVE ( 'NONE', #3764, #2804, #5175, .T. ) ;
#9144 = FACE_OUTER_BOUND ( 'NONE', #9800, .T. ) ;
#9145 = CARTESIAN_POINT ( 'NONE',  ( -21.91899880027261460, 100.0000000000000000, -9.705014769524845875 ) ) ;
#9146 = CYLINDRICAL_SURFACE ( 'NONE', #7554, 2.500000000000000000 ) ;
#9147 = EDGE_CURVE ( 'NONE', #5722, #7134, #6878, .T. ) ;
#9148 = ORIENTED_EDGE ( 'NONE', *, *, #1606, .F. ) ;
#9149 = CARTESIAN_POINT ( 'NONE',  ( 4.887668416326221177, 99.50000000000001421, -23.70513093767710089 ) ) ;
#9150 = AXIS2_PLACEMENT_3D ( 'NONE', #116, #6497, #7368 ) ;
#9151 = CARTESIAN_POINT ( 'NONE',  ( -9.703070624755296135E-15, -4.837500000000001243, 2.500000000000000444 ) ) ;
#9152 = EDGE_LOOP ( 'NONE', ( #9597, #4833, #7003, #308 ) ) ;
#9153 = CARTESIAN_POINT ( 'NONE',  ( 2.500000000000000444, -1.162499999999999645, 1.443375672974063439 ) ) ;
#9154 = DIRECTION ( 'NONE',  ( -0.2907782774943305504, 0.000000000000000000, -0.9567904646982169359 ) ) ;
#9155 = CARTESIAN_POINT ( 'NONE',  ( 2.256430356249999658, -0.4406249993854829961, -1.302750673588581432 ) ) ;
#9156 = CARTESIAN_POINT ( 'NONE',  ( 27.43301270000000258, 3.499999998907525445, -11.36312591709336139 ) ) ;
#9157 = EDGE_LOOP ( 'NONE', ( #928, #9267, #5770, #7592 ) ) ;
#9158 = CARTESIAN_POINT ( 'NONE',  ( -0.6698729810778054627, -1.257596189432333977, 2.500000000000000000 ) ) ;
#9159 = AXIS2_PLACEMENT_3D ( 'NONE', #6731, #302, #9872 ) ;
#9160 = DIRECTION ( 'NONE',  ( -0.5190318799156541374, 0.000000000000000000, -0.8547548816071318667 ) ) ;
#9161 = CARTESIAN_POINT ( 'NONE',  ( -21.11719860449141351, 99.99999999999995737, -9.425423427278841970 ) ) ;
#9162 = CARTESIAN_POINT ( 'NONE',  ( 0.000000000000000000, 0.000000000000000000, 0.000000000000000000 ) ) ;
#9163 = EDGE_LOOP ( 'NONE', ( #6976, #8728, #3348, #2792 ) ) ;
#9164 = CARTESIAN_POINT ( 'NONE',  ( -1.595409442497313560E-16, -0.7031249993854827851, -2.605501347177161087 ) ) ;
#9165 = CARTESIAN_POINT ( 'NONE',  ( -15.34161522349497808, 99.49999999999998579, 15.37783959465231121 ) ) ;
#9166 = CARTESIAN_POINT ( 'NONE',  ( -16.60513711880303234, 99.99999999999997158, 15.15667007515659748 ) ) ;
#9167 = FACE_OUTER_BOUND ( 'NONE', #8149, .T. ) ;
#9168 = CARTESIAN_POINT ( 'NONE',  ( -21.45221949983897858, 100.0000000000000000, -9.661157428473494235 ) ) ;
#9169 = VERTEX_POINT ( 'NONE', #4472 ) ;
#9170 = CARTESIAN_POINT ( 'NONE',  ( 4.750280232731688201, 100.0000000000000284, -24.05275076595185624 ) ) ;
#9171 = B_SPLINE_CURVE_WITH_KNOTS ( 'NONE', 3,
 ( #4017, #5639, #29, #1796, #1017, #5591, #8830, #140, #3283, #7303, #875, #4943, #7393, #2395, #185 ),
 .UNSPECIFIED., .F., .F.,
 ( 4, 1, 1, 1, 1, 1, 1, 1, 1, 1, 1, 1, 4 ),
 ( 0.000000000000000000, 0.08490232564366416435, 0.1680779112633816463, 0.2506304657828534177, 0.3338427399641299420, 0.4169763759729993580, 0.4990117930239920674, 0.5811067191809071719, 0.6656374296971073745, 0.7500328835558887075, 0.8331455368193440014, 0.9159638734519762737, 1.000000000000000000 ),
 .UNSPECIFIED. ) ;
#9172 = CARTESIAN_POINT ( 'NONE',  ( 2.256430356249999658, -2.690624999385482941, -1.302750673588581432 ) ) ;
#9173 = VERTEX_POINT ( 'NONE', #3031 ) ;
#9174 = DIRECTION ( 'NONE',  ( -0.2907782774943305504, 0.000000000000000000, -0.9567904646982169359 ) ) ;
#9175 = CARTESIAN_POINT ( 'NONE',  ( 9.877377282685029372E-16, -1.631249998770965659, 2.500000000000000000 ) ) ;
#9176 = CARTESIAN_POINT ( 'NONE',  ( 3.750007936853901658, 99.50000000000001421, -22.95001988029826734 ) ) ;
#9177 = CARTESIAN_POINT ( 'NONE',  ( -27.00000000000000355, 3.399999997815049912, -3.306546357697854128E-15 ) ) ;
#9178 = ADVANCED_FACE ( 'NONE', ( #4584 ), #443, .T. ) ;
#9179 = CARTESIAN_POINT ( 'NONE',  ( -16.81182640597031508, 100.0000000000000000, 16.36129326314865295 ) ) ;
#9180 = CARTESIAN_POINT ( 'NONE',  ( 3.386276725104728769, 99.50000000000001421, -24.01678749451497907 ) ) ;
#9181 =( BOUNDED_CURVE ( )  B_SPLINE_CURVE ( 2, ( #6363, #9698, #8087, #2385, #9557, #8918, #3225, #3127, #4108 ),
 .UNSPECIFIED., .F., .T. ) 
 B_SPLINE_CURVE_WITH_KNOTS ( ( 3, 2, 2, 2, 3 ),
 ( 0.1785714285714285754, 0.1964285714285714246, 0.2142857142857142738, 0.2321428571428571508, 0.2500000000000000000 ),
 .UNSPECIFIED. ) 
 CURVE ( )  GEOMETRIC_REPRESENTATION_ITEM ( )  RATIONAL_B_SPLINE_CURVE ( ( 1.000000000000000000, 0.9238795325112867385, 1.000000000000000000, 0.9238795325112867385, 1.000000000000000000, 0.9238795325112867385, 1.000000000000000000, 0.9238795325112867385, 1.000000000000000000 ) ) 
 REPRESENTATION_ITEM ( '' )  );
#9182 = VERTEX_POINT ( 'NONE', #6207 ) ;
#9183 = DIRECTION ( 'NONE',  ( -0.000000000000000000, 1.000000000000000000, -0.000000000000000000 ) ) ;
#9184 = CARTESIAN_POINT ( 'NONE',  ( -19.39806930854667755, 3.049999998907525711, -19.39806930854668110 ) ) ;
#9185 = DIRECTION ( 'NONE',  ( -1.000000000000000000, -0.000000000000000000, -0.000000000000000000 ) ) ;
#9186 = CARTESIAN_POINT ( 'NONE',  ( 9.723125805078051798, 99.50000000000000000, 21.50134635983626907 ) ) ;
#9187 = EDGE_CURVE ( 'NONE', #6069, #7809, #9405, .T. ) ;
#9188 = ORIENTED_EDGE ( 'NONE', *, *, #9518, .T. ) ;
#9189 = CARTESIAN_POINT ( 'NONE',  ( -21.11719860449141351, 100.0000000000000284, -9.425423427278841970 ) ) ;
#9190 = CARTESIAN_POINT ( 'NONE',  ( 8.751508028230254865, 99.99999999999998579, 19.58480916780017722 ) ) ;
#9191 = CARTESIAN_POINT ( 'NONE',  ( 27.00000000000000355, 3.200000000000000178, 0.000000000000000000 ) ) ;
#9192 = FACE_OUTER_BOUND ( 'NONE', #9253, .T. ) ;
#9193 = FACE_OUTER_BOUND ( 'NONE', #5200, .T. ) ;
#9194 = ORIENTED_EDGE ( 'NONE', *, *, #85, .F. ) ;
#9195 = CARTESIAN_POINT ( 'NONE',  ( -15.98972951825121669, 99.49999999999997158, 15.19400804711857411 ) ) ;
#9196 = CARTESIAN_POINT ( 'NONE',  ( -11.36312591709337561, 2.499999998907525445, 27.43301269999999548 ) ) ;
#9197 = ORIENTED_EDGE ( 'NONE', *, *, #7406, .T. ) ;
#9198 = CARTESIAN_POINT ( 'NONE',  ( 5.302876193624534821E-16, -2.137499999999999734, 2.886751345948128655 ) ) ;
#9199 = CARTESIAN_POINT ( 'NONE',  ( 3.106448761625311139, 99.49999999999998579, -21.38062202216113761 ) ) ;
#9200 = CARTESIAN_POINT ( 'NONE',  ( -2.256430356250000102, -2.540624999385482141, -1.302750673588580321 ) ) ;
#9201 = CARTESIAN_POINT ( 'NONE',  ( 27.43301269999999548, 2.599999998907525089, 11.36312591709337738 ) ) ;
#9202 = CARTESIAN_POINT ( 'NONE',  ( 1.653273178848927064E-15, 1.800000000000000266, -27.00000000000000355 ) ) ;
#9203 = CARTESIAN_POINT ( 'NONE',  ( 8.536201443755420115, 100.0000000000000284, 19.63502355897212581 ) ) ;
#9204 = CARTESIAN_POINT ( 'NONE',  ( 3.810791133452845703, 100.0000000000000568, -24.33305202239136733 ) ) ;
#9205 = CARTESIAN_POINT ( 'NONE',  ( 3.349514647153394975, 99.99999999999998579, -23.95461210612682024 ) ) ;
#9206 = CARTESIAN_POINT ( 'NONE',  ( -2.256430356250000102, -0.1406249993854829794, 0.000000000000000000 ) ) ;
#9207 = DIRECTION ( 'NONE',  ( -0.4980973490458728836, -0.08715574274765837404, 0.8627299156628208676 ) ) ;
#9208 = CARTESIAN_POINT ( 'NONE',  ( -1.249999999999998224, -1.218749998770965792, 2.165063509461097713 ) ) ;
#9209 = CARTESIAN_POINT ( 'NONE',  ( 11.36312591709336850, 0.8999999989075253559, 27.43301269999999903 ) ) ;
#9210 = VERTEX_POINT ( 'NONE', #2233 ) ;
#9211 = CARTESIAN_POINT ( 'NONE',  ( 19.09188309203678813, 4.899999999999999467, -19.09188309203678813 ) ) ;
#9212 = AXIS2_PLACEMENT_3D ( 'NONE', #4924, #6545, #8025 ) ;
#9213 = ADVANCED_FACE ( 'NONE', ( #5436, #556 ), #1448, .F. ) ;
#9214 = CARTESIAN_POINT ( 'NONE',  ( 3.986298408513477387, 99.50000000000002842, -22.53092616755505162 ) ) ;
#9215 = CARTESIAN_POINT ( 'NONE',  ( 0.000000000000000000, 5.000000000000000000, 0.000000000000000000 ) ) ;
#9216 = VERTEX_POINT ( 'NONE', #3748 ) ;
#9217 = CARTESIAN_POINT ( 'NONE',  ( 4.871887406949175769, 99.99999999999995737, -23.77896509604281405 ) ) ;
#9218 = CARTESIAN_POINT ( 'NONE',  ( -2.256430356250000102, -2.953124999385482674, 0.000000000000000000 ) ) ;
#9219 = EDGE_LOOP ( 'NONE', ( #3078, #34, #4234, #5715 ) ) ;
#9220 = CARTESIAN_POINT ( 'NONE',  ( 4.723706824522782455, 99.50000000000000000, -24.08630974238606370 ) ) ;
#9221 = CARTESIAN_POINT ( 'NONE',  ( 0.000000000000000000, 0.000000000000000000, -2.500000000000000000 ) ) ;
#9222 = CARTESIAN_POINT ( 'NONE',  ( -2.256430356250000102, -0.2531249993854829405, 0.000000000000000000 ) ) ;
#9223 = CARTESIAN_POINT ( 'NONE',  ( 2.936358689207804851, 100.0000000000000000, -23.74786164940363875 ) ) ;
#9224 = ORIENTED_EDGE ( 'NONE', *, *, #7543, .F. ) ;
#9225 = VECTOR ( 'NONE', #6697, 1000.000000000000000 ) ;
#9226 = ORIENTED_EDGE ( 'NONE', *, *, #2174, .F. ) ;
#9227 = CARTESIAN_POINT ( 'NONE',  ( 3.948639947730041566, 99.49999999999998579, -21.07692942975820927 ) ) ;
#9228 = CARTESIAN_POINT ( 'NONE',  ( -16.88522588321459494, 100.0000000000000284, 16.18266969485829421 ) ) ;
#9229 = CARTESIAN_POINT ( 'NONE',  ( 0.000000000000000000, -5.000000000000000000, 0.000000000000000000 ) ) ;
#9230 = ORIENTED_EDGE ( 'NONE', *, *, #9274, .T. ) ;
#9231 = CARTESIAN_POINT ( 'NONE',  ( 19.09188309203678102, 1.299999997815050268, 19.09188309203678813 ) ) ;
#9232 = CARTESIAN_POINT ( 'NONE',  ( -5.039362679103552881E-15, 4.949999998907525622, 27.43301270000000258 ) ) ;
#9233 = CARTESIAN_POINT ( 'NONE',  ( 4.909381318607588973, 100.0000000000000000, -23.54377677363417121 ) ) ;
#9234 = CARTESIAN_POINT ( 'NONE',  ( 9.766630880609509902, 100.0000000000000142, 21.37293705761699059 ) ) ;
#9235 = CARTESIAN_POINT ( 'NONE',  ( -21.99154324187120579, 100.0000000000000142, -9.362771248264911250 ) ) ;
#9236 = CARTESIAN_POINT ( 'NONE',  ( 4.688812652749139609, 99.50000000000001421, -24.54863390154074310 ) ) ;
#9237 = DIRECTION ( 'NONE',  ( -0.000000000000000000, -1.000000000000000000, -0.000000000000000000 ) ) ;
#9238 =( BOUNDED_CURVE ( )  B_SPLINE_CURVE ( 2, ( #6405, #4052, #9693, #2483, #7234, #5676, #127, #10341, #7287 ),
 .UNSPECIFIED., .F., .F. ) 
 B_SPLINE_CURVE_WITH_KNOTS ( ( 3, 2, 2, 2, 3 ),
 ( 0.8541666666666667407, 0.8611111111111111605, 0.8750000000000000000, 0.8888888888888888395, 0.8958333333333333703 ),
 .UNSPECIFIED. ) 
 CURVE ( )  GEOMETRIC_REPRESENTATION_ITEM ( )  RATIONAL_B_SPLINE_CURVE ( ( 0.9330127018922192983, 0.9330127018922198534, 1.000000000000000000, 0.8660254037844387076, 1.000000000000000000, 0.8660254037844387076, 1.000000000000000000, 0.9330127018922187432, 0.9330127018922192983 ) ) 
 REPRESENTATION_ITEM ( '' )  );
#9239 = CARTESIAN_POINT ( 'NONE',  ( -16.57687742313193269, 99.50000000000002842, 15.91855687263828756 ) ) ;
#9240 = CARTESIAN_POINT ( 'NONE',  ( 1.045839947578414805E-15, -0.5625000000000001110, -2.500000000000000000 ) ) ;
#9241 = ORIENTED_EDGE ( 'NONE', *, *, #10227, .F. ) ;
#9242 = CARTESIAN_POINT ( 'NONE',  ( -16.36470918167357169, 99.50000000000000000, 16.79054296464299867 ) ) ;
#9243 = CARTESIAN_POINT ( 'NONE',  ( -19.39806930854668465, 2.449999998907525622, 19.39806930854667755 ) ) ;
#9244 = ORIENTED_EDGE ( 'NONE', *, *, #5457, .T. ) ;
#9245 = ADVANCED_FACE ( 'NONE', ( #3857 ), #90, .T. ) ;
#9246 = CARTESIAN_POINT ( 'NONE',  ( -1.250000000000000222, -2.324999999999999734, -2.165063509461096825 ) ) ;
#9247 = APPLICATION_PROTOCOL_DEFINITION ( 'draft international standard', 'automotive_design', 1998, #2270 ) ;
#9248 = CARTESIAN_POINT ( 'NONE',  ( 9.182805720491336032, 99.50000000000000000, 20.00174565872165289 ) ) ;
#9249 = CARTESIAN_POINT ( 'NONE',  ( 0.000000000000000000, -20.00000000000000000, 0.000000000000000000 ) ) ;
#9250 = CARTESIAN_POINT ( 'NONE',  ( -1.595409442497313560E-16, -0.8156249993854829405, -2.605501347177161087 ) ) ;
#9251 = CARTESIAN_POINT ( 'NONE',  ( 19.39806930854667399, 4.949999998907525622, 19.39806930854668465 ) ) ;
#9252 = CARTESIAN_POINT ( 'NONE',  ( -5.039362679103552881E-15, 2.549999998907525267, 27.43301270000000258 ) ) ;
#9254 = VERTEX_POINT ( 'NONE', #4744 ) ;
#9253 = EDGE_LOOP ( 'NONE', ( #113, #2343 ) ) ;
#9255 = PRODUCT_DEFINITION_CONTEXT ( 'detailed design', #8548, 'design' ) ;
#9256 = CARTESIAN_POINT ( 'NONE',  ( -15.17782247516205274, 99.99999999999998579, 15.06300032623928686 ) ) ;
#9257 = DIRECTION ( 'NONE',  ( 0.9985355274883277454, 0.000000000000000000, -0.05409991075415104128 ) ) ;
#9258 = CARTESIAN_POINT ( 'NONE',  ( 7.783718120363267268, 99.99999999999998579, 21.09473326129887027 ) ) ;
#9259 = PRODUCT_DEFINITION_SHAPE ( 'NONE', 'NONE',  #10373 ) ;
#9260 = CARTESIAN_POINT ( 'NONE',  ( -15.49723655759404295, 99.99999999999997158, 15.26389171799780264 ) ) ;
#9261 = CARTESIAN_POINT ( 'NONE',  ( -1.128215178125000273, -0.6656249993854830294, -1.954126010382871259 ) ) ;
#9262 = CARTESIAN_POINT ( 'NONE',  ( -21.29537297865864431, 99.50000000000000000, -11.39144590536739976 ) ) ;
#9263 = VERTEX_POINT ( 'NONE', #1500 ) ;
#9264 = CARTESIAN_POINT ( 'NONE',  ( -2.378215178125000495, -0.07031249969274147582, 0.000000000000000000 ) ) ;
#9265 = CARTESIAN_POINT ( 'NONE',  ( 1.679787559701184688E-15, 2.049999998907525711, -27.43301270000000258 ) ) ;
#9266 = SURFACE_STYLE_USAGE ( .BOTH. , #10054 ) ;
#9267 = ORIENTED_EDGE ( 'NONE', *, *, #6476, .F. ) ;
#9268 = CARTESIAN_POINT ( 'NONE',  ( -15.07178375341841559, 99.50000000000001421, 15.16157792772069968 ) ) ;
#9269 = CARTESIAN_POINT ( 'NONE',  ( 26.99999999999999645, 1.550000000000000044, 11.18376618407358691 ) ) ;
#9270 = CARTESIAN_POINT ( 'NONE',  ( 6.477538756577482459, 99.50000000000000000, 20.49684993083915430 ) ) ;
#9271 = ORIENTED_EDGE ( 'NONE', *, *, #8781, .T. ) ;
#9272 = AXIS2_PLACEMENT_3D ( 'NONE', #736, #4132, #8893 ) ;
#9273 = CARTESIAN_POINT ( 'NONE',  ( -15.91084591538827198, 99.50000000000001421, 16.65047278764667027 ) ) ;
#9274 = EDGE_CURVE ( 'NONE', #1968, #4141, #1895, .T. ) ;
#9275 = CARTESIAN_POINT ( 'NONE',  ( 1.128215178124999607, -2.653124999385482408, -1.954126010382871259 ) ) ;
#9276 = ORIENTED_EDGE ( 'NONE', *, *, #1465, .F. ) ;
#9277 = EDGE_CURVE ( 'NONE', #9319, #9715, #3801, .T. ) ;
#9278 = CARTESIAN_POINT ( 'NONE',  ( -22.12191435419165941, 99.99999999999998579, -9.834338183724410598 ) ) ;
#9279 = CARTESIAN_POINT ( 'NONE',  ( -15.07178375341841381, 100.0000000000000000, 16.66969090848992607 ) ) ;
#9280 = DIRECTION ( 'NONE',  ( -0.9854855627156250408, 0.000000000000000000, -0.1697592580069431922 ) ) ;
#9281 = CARTESIAN_POINT ( 'NONE',  ( -1.128215178125000273, -0.7781249993854828517, -1.954126010382871259 ) ) ;
#9282 = CARTESIAN_POINT ( 'NONE',  ( 2.940631318607589417, 100.0000000000000000, -23.77584808773673331 ) ) ;
#9283 = CIRCLE ( 'NONE', #8635, 27.00000000000000000 ) ;
#9284 = ORIENTED_EDGE ( 'NONE', *, *, #2500, .T. ) ;
#9285 = CARTESIAN_POINT ( 'NONE',  ( 3.861186820804014097, 99.50000000000004263, -21.07288982789904708 ) ) ;
#9286 = CARTESIAN_POINT ( 'NONE',  ( -16.70213339477928471, 99.99999999999998579, 16.52464093453885852 ) ) ;
#9287 = LINE ( 'NONE', #2854, #7804 ) ;
#9288 = ORIENTED_EDGE ( 'NONE', *, *, #5103, .T. ) ;
#9289 = CARTESIAN_POINT ( 'NONE',  ( 24.00000000000000711, 73.81339255365637086, -2.939152317953649078E-15 ) ) ;
#9290 = CARTESIAN_POINT ( 'NONE',  ( -11.36312591709335962, 2.999999998907524557, -27.43301270000000258 ) ) ;
#9291 = CARTESIAN_POINT ( 'NONE',  ( -2.256430356249999214, -1.903124999385482852, 1.302750673588581876 ) ) ;
#9292 = PLANE ( 'NONE',  #5086 ) ;
#9293 = VERTEX_POINT ( 'NONE', #873 ) ;
#9294 = CARTESIAN_POINT ( 'NONE',  ( -2.500000000000000000, -0.8437499987709659033, 0.000000000000000000 ) ) ;
#9295 = CARTESIAN_POINT ( 'NONE',  ( 5.242860087038358152, 99.50000000000002842, -23.52699316036146371 ) ) ;
#9296 = CARTESIAN_POINT ( 'NONE',  ( 0.000000000000000000, 0.000000000000000000, -0.4999999999999953371 ) ) ;
#9297 = DIRECTION ( 'NONE',  ( 0.000000000000000000, -1.000000000000000000, 0.000000000000000000 ) ) ;
#9298 = ORIENTED_EDGE ( 'NONE', *, *, #3321, .T. ) ;
#9299 = CARTESIAN_POINT ( 'NONE',  ( -15.91768310440539658, 99.50000000000002842, 15.18344740530786652 ) ) ;
#9300 = AXIS2_PLACEMENT_3D ( 'NONE', #2, #7121, #3253 ) ;
#9301 = CARTESIAN_POINT ( 'NONE',  ( -11.36312591709335962, 0.5999999989075253115, -27.43301270000000258 ) ) ;
#9302 = CIRCLE ( 'NONE', #440, 1.324999999999999734 ) ;
#9303 = PRESENTATION_LAYER_ASSIGNMENT (  '', '', ( #7982 ) ) ;
#9304 = CARTESIAN_POINT ( 'NONE',  ( -1.250000000000000222, -0.5250000000000000222, -2.165063509461096825 ) ) ;
#9305 = APPLICATION_PROTOCOL_DEFINITION ( 'draft international standard', 'automotive_design', 1998, #4600 ) ;
#9306 = CARTESIAN_POINT ( 'NONE',  ( -22.43208371148383762, 99.50000000000000000, -9.654966607469265938 ) ) ;
#9307 = CARTESIAN_POINT ( 'NONE',  ( 2.901827748664965068, 99.49999999999998579, -21.68759887446373469 ) ) ;
#9308 = CARTESIAN_POINT ( 'NONE',  ( -2.256430356250000102, -2.953124999385482674, 0.000000000000000000 ) ) ;
#9309 = CARTESIAN_POINT ( 'NONE',  ( -16.84090648038580085, 99.49999999999998579, 15.49469789757679727 ) ) ;
#9310 = CARTESIAN_POINT ( 'NONE',  ( -19.39806930854667755, 3.049999998907525711, -19.39806930854668110 ) ) ;
#9312 = ORIENTED_EDGE ( 'NONE', *, *, #820, .F. ) ;
#9311 = ORIENTED_EDGE ( 'NONE', *, *, #8817, .F. ) ;
#9313 = EDGE_CURVE ( 'NONE', #2748, #7711, #7249, .T. ) ;
#9314 = B_SPLINE_CURVE_WITH_KNOTS ( 'NONE', 3,
 ( #2979, #8632, #10026, #1236 ),
 .UNSPECIFIED., .F., .F.,
 ( 4, 4 ),
 ( 0.000000000000000000, 1.000000000000000000 ),
 .UNSPECIFIED. ) ;
#9315 = CARTESIAN_POINT ( 'NONE',  ( 9.063633472794011325, 99.99999999999998579, 19.59517414759687526 ) ) ;
#9316 = CARTESIAN_POINT ( 'NONE',  ( 8.105710127743357418, 99.50000000000000000, 20.44429669797862559 ) ) ;
#9317 = CARTESIAN_POINT ( 'NONE',  ( -16.42071764973191250, 99.50000000000001421, 16.76105279315999042 ) ) ;
#9318 = CARTESIAN_POINT ( 'NONE',  ( 3.282077632710153292, 100.0000000000000000, -23.74569985055724786 ) ) ;
#9319 = VERTEX_POINT ( 'NONE', #7150 ) ;
#9320 = CARTESIAN_POINT ( 'NONE',  ( -1.595409442497313560E-16, -1.603124999385482807, -2.605501347177161087 ) ) ;
#9321 = CARTESIAN_POINT ( 'NONE',  ( -2.499999999999999112, -5.306249998770965703, 1.443375672974065882 ) ) ;
#9322 = ORIENTED_EDGE ( 'NONE', *, *, #1009, .F. ) ;
#9323 = FACE_OUTER_BOUND ( 'NONE', #400, .T. ) ;
#9324 = CARTESIAN_POINT ( 'NONE',  ( -11.36312591709335962, 2.899999998907525356, -27.43301270000000258 ) ) ;
#9325 = ORIENTED_EDGE ( 'NONE', *, *, #9664, .F. ) ;
#9326 = CARTESIAN_POINT ( 'NONE',  ( -15.70584307919286893, 99.99999999999995737, 14.84247401567675162 ) ) ;
#9327 = CARTESIAN_POINT ( 'NONE',  ( -27.00000000000000355, 0.4000000000000000222, -3.306546357697854128E-15 ) ) ;
#9328 = VECTOR ( 'NONE', #10337, 1000.000000000000000 ) ;
#9329 = CARTESIAN_POINT ( 'NONE',  ( 9.304660012616079001, 100.0000000000000284, 20.07619068507570859 ) ) ;
#9330 = ORIENTED_EDGE ( 'NONE', *, *, #2246, .F. ) ;
#9331 = ORIENTED_EDGE ( 'NONE', *, *, #9777, .T. ) ;
#9332 = EDGE_CURVE ( 'NONE', #9263, #3256, #10353, .T. ) ;
#9333 = CARTESIAN_POINT ( 'NONE',  ( -16.45635306197508996, 99.99999999999995737, 15.51056558312563105 ) ) ;
#9334 = FACE_OUTER_BOUND ( 'NONE', #5191, .T. ) ;
#9335 = EDGE_LOOP ( 'NONE', ( #9614, #1837, #1545, #3813 ) ) ;
#9336 = CARTESIAN_POINT ( 'NONE',  ( -1.128215178124998497, -1.528124999385482852, 1.954126010382872147 ) ) ;
#9337 = ORIENTED_EDGE ( 'NONE', *, *, #1160, .F. ) ;
#9338 = VECTOR ( 'NONE', #4265, 1000.000000000000000 ) ;
#9339 = CARTESIAN_POINT ( 'NONE',  ( -22.57971655928959365, 99.50000000000000000, -10.84768434062017839 ) ) ;
#9340 = CARTESIAN_POINT ( 'NONE',  ( -19.39806930854668465, 0.7499999989075252227, 19.39806930854667755 ) ) ;
#9341 = CARTESIAN_POINT ( 'NONE',  ( -21.38163724633288965, 99.50000000000005684, -9.681902434707239991 ) ) ;
#9342 = PRODUCT_RELATED_PRODUCT_CATEGORY ( 'part', '', ( #7269 ) ) ;
#9343 = CARTESIAN_POINT ( 'NONE',  ( 1.128215178124999607, -2.203124999385482674, -1.954126010382871259 ) ) ;
#9344 = EDGE_CURVE ( 'NONE', #3170, #7765, #5487, .T. ) ;
#9345 = CARTESIAN_POINT ( 'NONE',  ( -19.75840245672548789, 99.50000000000000000, -8.735905494466331689 ) ) ;
#9346 = EDGE_CURVE ( 'NONE', #1470, #2280, #8142, .T. ) ;
#9347 = DIRECTION ( 'NONE',  ( 0.000000000000000000, -1.000000000000000000, 0.000000000000000000 ) ) ;
#9348 = CARTESIAN_POINT ( 'NONE',  ( -16.74216497804568604, 100.0000000000000142, 15.31795814478965312 ) ) ;
#9349 = CARTESIAN_POINT ( 'NONE',  ( 9.877377282685029372E-16, -3.037499999999999201, 2.500000000000000000 ) ) ;
#9350 = VERTEX_POINT ( 'NONE', #8095 ) ;
#9351 = CARTESIAN_POINT ( 'NONE',  ( 0.6698729810778075722, -1.217403810567665667, 2.499999999999999556 ) ) ;
#9352 = CARTESIAN_POINT ( 'NONE',  ( 1.034219503716432668E-14, -4.162500000000000533, -2.500000000000000000 ) ) ;
#9353 = CARTESIAN_POINT ( 'NONE',  ( -1.128215178124998497, -0.5156249993854828961, 1.954126010382872147 ) ) ;
#9354 = CARTESIAN_POINT ( 'NONE',  ( 9.676361905416721143, 100.0000000000000000, 21.63547735782115566 ) ) ;
#9355 = B_SPLINE_SURFACE_WITH_KNOTS ( 'NONE', 3, 1, ( 
 ( #8059, #894 ),
 ( #3299, #9145 ),
 ( #2609, #4328 ),
 ( #2656, #1812 ),
 ( #7512, #9821 ),
 ( #8204, #202 ),
 ( #7361, #2564 ),
 ( #3491, #5846 ),
 ( #351, #9041 ),
 ( #3387, #1034 ),
 ( #5953, #9770 ),
 ( #6579, #156 ),
 ( #5755, #5159 ),
 ( #5800, #7408 ),
 ( #2709, #5898 ),
 ( #8256, #5004 ),
 ( #249, #8991 ),
 ( #1859, #4229 ),
 ( #2763, #3436 ) ),
 .UNSPECIFIED., .F., .F., .F.,
 ( 4, 1, 1, 1, 1, 1, 1, 1, 1, 1, 1, 1, 1, 1, 1, 1, 4 ),
 ( 2, 2 ),
 ( 0.000000000000000000, 0.06505403082392276215, 0.1283503816230405770, 0.1902281050068566903, 0.2509397092642763338, 0.3119571365542418429, 0.3738829716944830350, 0.4367040802691206092, 0.5009896104483916313, 0.5655726868558689224, 0.6286067690057803858, 0.6898677555008378981, 0.7506620835893632604, 0.8110632348575060879, 0.8726242918051292374, 0.9355756365154705989, 0.9999999999999998890 ),
 ( 0.000000000000000000, 1.000000000000000000 ),
 .UNSPECIFIED. ) ;
#9356 = ORIENTED_EDGE ( 'NONE', *, *, #1606, .T. ) ;
#9357 = EDGE_CURVE ( 'NONE', #1260, #4596, #5637, .T. ) ;
#9358 = CARTESIAN_POINT ( 'NONE',  ( -7.500000000000000888, 104.5000000000000142, 3.000000000000000000 ) ) ;
#9359 = CARTESIAN_POINT ( 'NONE',  ( 8.961048541867139505, 100.0000000000000142, 19.57961630251783092 ) ) ;
#9360 = CARTESIAN_POINT ( 'NONE',  ( -16.07368679829020763, 99.50000000000000000, 17.11560437002838952 ) ) ;
#9361 = CARTESIAN_POINT ( 'NONE',  ( -16.49419651247312046, 99.49999999999998579, 15.57134447358898477 ) ) ;
#9362 = ORIENTED_EDGE ( 'NONE', *, *, #10165, .T. ) ;
#9363 = CARTESIAN_POINT ( 'NONE',  ( -4.357666448243394824E-15, -2.981249998770965526, 2.500000000000000000 ) ) ;
#9364 = CARTESIAN_POINT ( 'NONE',  ( -11.36312591709335962, 1.399999998907525578, -27.43301270000000258 ) ) ;
#9365 = EDGE_LOOP ( 'NONE', ( #6550, #6840, #4324, #6316 ) ) ;
#9366 = CARTESIAN_POINT ( 'NONE',  ( 5.302876193624534821E-16, -3.487499999999999822, 2.886751345948128655 ) ) ;
#9367 =( LENGTH_UNIT ( ) NAMED_UNIT ( * ) SI_UNIT ( .MILLI., .METRE. ) );
#9368 = CARTESIAN_POINT ( 'NONE',  ( -1.868473738487927527, -5.035679442772306835, -1.567817502008199249 ) ) ;
#9369 = CARTESIAN_POINT ( 'NONE',  ( 2.256430356249999658, -2.240624999385482319, -1.302750673588581432 ) ) ;
#9370 = DIRECTION ( 'NONE',  ( 1.000000000000000000, 0.000000000000000000, 0.000000000000000000 ) ) ;
#9371 = CARTESIAN_POINT ( 'NONE',  ( -19.39806930854668465, 2.449999998907525622, 19.39806930854667755 ) ) ;
#9372 = ORIENTED_EDGE ( 'NONE', *, *, #5394, .F. ) ;
#9373 = CARTESIAN_POINT ( 'NONE',  ( -16.12311789350856017, 100.0000000000000000, 14.86696503675854686 ) ) ;
#9374 = LINE ( 'NONE', #7014, #2135 ) ;
#9375 = CARTESIAN_POINT ( 'NONE',  ( 2.864934851235464208, 99.50000000000000000, -21.80148171563692827 ) ) ;
#9376 = CARTESIAN_POINT ( 'NONE',  ( 0.000000000000000000, 0.000000000000000000, 0.000000000000000000 ) ) ;
#9377 = CIRCLE ( 'NONE', #4183, 27.00000000000000355 ) ;
#9378 = CARTESIAN_POINT ( 'NONE',  ( 2.256430356249999658, -1.228124999385483029, -1.302750673588581432 ) ) ;
#9379 = CARTESIAN_POINT ( 'NONE',  ( 4.433602057339688152, 100.0000000000000000, -21.25644978738549540 ) ) ;
#9380 = ORIENTED_EDGE ( 'NONE', *, *, #2624, .F. ) ;
#9381 = FACE_OUTER_BOUND ( 'NONE', #8509, .T. ) ;
#9382 = CARTESIAN_POINT ( 'NONE',  ( 11.36312591709336139, 2.799999998907525267, -27.43301270000000258 ) ) ;
#9383 = EDGE_LOOP ( 'NONE', ( #4685, #267, #662, #8283 ) ) ;
#9384 = LINE ( 'NONE', #10282, #236 ) ;
#9385 = CARTESIAN_POINT ( 'NONE',  ( 3.207057600658871355, 99.50000000000000000, -22.07913334414698880 ) ) ;
#9386 = CARTESIAN_POINT ( 'NONE',  ( 9.357295078982289738, 100.0000000000000711, 20.12145687760884627 ) ) ;
#9387 = ORIENTED_EDGE ( 'NONE', *, *, #7878, .T. ) ;
#9388 = EDGE_LOOP ( 'NONE', ( #2872, #4908, #226, #5476 ) ) ;
#9389 = CARTESIAN_POINT ( 'NONE',  ( -15.32348647777738826, 99.50000000000000000, 15.39505148541300450 ) ) ;
#9390 = CARTESIAN_POINT ( 'NONE',  ( -15.37123125604856710, 99.50000000000001421, 16.48683530611566539 ) ) ;
#9391 = CARTESIAN_POINT ( 'NONE',  ( -1.128215178125000273, -3.028124999385482408, -1.954126010382871259 ) ) ;
#9392 = EDGE_LOOP ( 'NONE', ( #6526, #7093 ) ) ;
#9393 = ORIENTED_EDGE ( 'NONE', *, *, #9851, .T. ) ;
#9394 = PLANE ( 'NONE',  #1456 ) ;
#9395 = CIRCLE ( 'NONE', #1045, 20.00000000000000000 ) ;
#9396 = CARTESIAN_POINT ( 'NONE',  ( 0.000000000000000000, 85.00000000000000000, 0.000000000000000000 ) ) ;
#9397 = EDGE_CURVE ( 'NONE', #1366, #9616, #8240, .T. ) ;
#9398 = CARTESIAN_POINT ( 'NONE',  ( -1.128215178125000273, -2.128124999385482496, -1.954126010382871259 ) ) ;
#9399 = CARTESIAN_POINT ( 'NONE',  ( 5.243816414761435674, 100.0000000000000284, -23.48558366465980995 ) ) ;
#9400 = VERTEX_POINT ( 'NONE', #4016 ) ;
#9401 = DIRECTION ( 'NONE',  ( -0.000000000000000000, -1.000000000000000000, 0.000000000000000000 ) ) ;
#9402 = AXIS2_PLACEMENT_3D ( 'NONE', #4992, #3418, #9907 ) ;
#9403 = CARTESIAN_POINT ( 'NONE',  ( -2.500000000000000000, -3.131249998770965437, -1.443375672974064106 ) ) ;
#9404 = CARTESIAN_POINT ( 'NONE',  ( -16.90689012439429462, 99.99999999999998579, 16.08742389234230785 ) ) ;
#9405 = LINE ( 'NONE', #6095, #786 ) ;
#9406 = VERTEX_POINT ( 'NONE', #7884 ) ;
#9407 = CARTESIAN_POINT ( 'NONE',  ( 25.15000000000000213, 3.079986699855593473E-15, 0.000000000000000000 ) ) ;
#9408 = CARTESIAN_POINT ( 'NONE',  ( 1.128215178124999607, -2.540624999385482585, -1.954126010382871259 ) ) ;
#9409 = VECTOR ( 'NONE', #8862, 1000.000000000000000 ) ;
#9410 = VERTEX_POINT ( 'NONE', #9661 ) ;
#9411 = CYLINDRICAL_SURFACE ( 'NONE', #7782, 30.00000000000000000 ) ;
#9412 = CARTESIAN_POINT ( 'NONE',  ( 4.401614252286283779, 99.50000000000002842, -24.65974366035752396 ) ) ;
#9413 = CARTESIAN_POINT ( 'NONE',  ( 0.000000000000000000, 70.00000000000000000, 0.000000000000000000 ) ) ;
#9414 = CARTESIAN_POINT ( 'NONE',  ( -16.49092618789450526, 99.50000000000000000, 16.26472549871478179 ) ) ;
#9415=STYLED_ITEM('',(#10408),#3102);
#9416 = EDGE_CURVE ( 'NONE', #7920, #4798, #3441, .T. ) ;
#9417 = ORIENTED_EDGE ( 'NONE', *, *, #9720, .T. ) ;
#9418 = LINE ( 'NONE', #7679, #7140 ) ;
#9419 = CIRCLE ( 'NONE', #3906, 27.00000000000000355 ) ;
#9420 = CARTESIAN_POINT ( 'NONE',  ( -11.36312591709337561, 0.8999999989075252449, 27.43301269999999548 ) ) ;
#9421 = ORIENTED_EDGE ( 'NONE', *, *, #7468, .T. ) ;
#9422 = ADVANCED_FACE ( 'NONE', ( #1657, #384 ), #9125, .F. ) ;
#9423 = CARTESIAN_POINT ( 'NONE',  ( -1.249999999999998224, -3.074999999999999734, 2.165063509461097713 ) ) ;
#9424 = CONTEXT_DEPENDENT_SHAPE_REPRESENTATION ( #5860, #9259 ) ;
#9425 = CARTESIAN_POINT ( 'NONE',  ( 3.023131990384279710, 100.0000000000000000, -21.47496011329876708 ) ) ;
#9426 = CARTESIAN_POINT ( 'NONE',  ( 1.128215178125001161, -1.003124999385482718, 1.954126010382870815 ) ) ;
#9427 = CARTESIAN_POINT ( 'NONE',  ( -5.039362679103552881E-15, 4.849999998907525089, 27.43301270000000258 ) ) ;
#9428 = CARTESIAN_POINT ( 'NONE',  ( 27.43301270000000258, 1.999999998907524779, -11.36312591709336139 ) ) ;
#9429 = STYLED_ITEM ( 'NONE', ( #5467 ), #3150 ) ;
#9430 = EDGE_LOOP ( 'NONE', ( #9090, #193, #7056, #6030 ) ) ;
#9431 = CARTESIAN_POINT ( 'NONE',  ( 8.429066232339796017, 100.0000000000000000, 19.67794530653910101 ) ) ;
#9432 = CARTESIAN_POINT ( 'NONE',  ( 4.202475441399873723, 100.0000000000000000, -24.35385978717689071 ) ) ;
#9433 = CARTESIAN_POINT ( 'NONE',  ( 3.399971579580567393, 99.50000000000000000, -21.57509867787664248 ) ) ;
#9434 = CARTESIAN_POINT ( 'NONE',  ( 7.486453019397995234, 99.50000000000000000, 23.81666162955709964 ) ) ;
#9435 = CARTESIAN_POINT ( 'NONE',  ( -1.128215178125000273, -1.565624999385482941, -1.954126010382871259 ) ) ;
#9436 = CARTESIAN_POINT ( 'NONE',  ( 4.743081672682207817, 100.0000000000000284, -21.60795120912350598 ) ) ;
#9437 = ORIENTED_EDGE ( 'NONE', *, *, #3903, .F. ) ;
#9438 = ORIENTED_EDGE ( 'NONE', *, *, #1008, .T. ) ;
#9439 = CARTESIAN_POINT ( 'NONE',  ( 2.256430356250000546, -1.753124999385482718, 1.302750673588579877 ) ) ;
#9440 = CARTESIAN_POINT ( 'NONE',  ( -11.36312591709335962, 2.099999998907525089, -27.43301270000000258 ) ) ;
#9441 =( LENGTH_UNIT ( ) NAMED_UNIT ( * ) SI_UNIT ( .MILLI., .METRE. ) );
#9442 = CARTESIAN_POINT ( 'NONE',  ( 0.000000000000000000, 85.00000000000000000, 0.000000000000000000 ) ) ;
#9443 = CARTESIAN_POINT ( 'NONE',  ( 11.18376618407357626, 2.250000000000000444, 27.00000000000000000 ) ) ;
#9444 = CARTESIAN_POINT ( 'NONE',  ( 8.757234875838378230, 99.50000000000000000, 19.92790116963689329 ) ) ;
#9445 = ORIENTED_EDGE ( 'NONE', *, *, #3027, .F. ) ;
#9446 = CARTESIAN_POINT ( 'NONE',  ( -15.10617644529808423, 99.50000000000002842, 15.98944417891004477 ) ) ;
#9447 = CARTESIAN_POINT ( 'NONE',  ( -15.55395551812965671, 100.0000000000000284, 16.59868653893595791 ) ) ;
#9448 = ORIENTED_EDGE ( 'NONE', *, *, #4537, .T. ) ;
#9449 = CARTESIAN_POINT ( 'NONE',  ( 2.256430356250000546, -3.665624999385482141, 1.302750673588579877 ) ) ;
#9450 = ORIENTED_EDGE ( 'NONE', *, *, #2670, .F. ) ;
#9451 = ORIENTED_EDGE ( 'NONE', *, *, #1453, .F. ) ;
#9452 = CARTESIAN_POINT ( 'NONE',  ( 19.39806930854667399, 1.749999998907525223, 19.39806930854668465 ) ) ;
#9453 = VECTOR ( 'NONE', #8547, 1000.000000000000000 ) ;
#9454 = DIRECTION ( 'NONE',  ( 0.000000000000000000, -1.000000000000000000, 0.000000000000000000 ) ) ;
#9455 = B_SPLINE_SURFACE_WITH_KNOTS ( 'NONE', 3, 1, ( 
 ( #4863, #3198 ),
 ( #9478, #7260 ),
 ( #5505, #888 ),
 ( #6380, #1515 ),
 ( #4708, #7901 ),
 ( #5601, #1617 ),
 ( #7114, #1756 ),
 ( #6670, #982 ),
 ( #4174, #7402 ),
 ( #7313, #4273 ),
 ( #3379, #6725 ),
 ( #4998, #7356 ),
 ( #5892, #151 ),
 ( #8198, #6574 ),
 ( #4322, #196 ),
 ( #5749, #9866 ),
 ( #6622, #2703 ),
 ( #5841, #8986 ),
 ( #345, #3486 ) ),
 .UNSPECIFIED., .F., .F., .F.,
 ( 4, 1, 1, 1, 1, 1, 1, 1, 1, 1, 1, 1, 1, 1, 1, 1, 4 ),
 ( 2, 2 ),
 ( 0.000000000000000000, 0.07039602572822099835, 0.1400447079551435658, 0.2099027554305550880, 0.2826152692239142783, 0.3556467613428230812, 0.4271065942619623468, 0.4986634349892335449, 0.5720141774457471184, 0.6112909118483191850, 0.6543288624652392471, 0.7009162800881839628, 0.7518538071550001645, 0.8072437197097745987, 0.8671654997918389896, 0.9315515937071113806, 1.000000000000000000 ),
 ( 0.000000000000000000, 1.000000000000000000 ),
 .UNSPECIFIED. ) ;
#9456 = CARTESIAN_POINT ( 'NONE',  ( -2.256430356249998770, -0.6656249993854829183, 1.302750673588581876 ) ) ;
#9457 = CARTESIAN_POINT ( 'NONE',  ( 5.098880966732203035, 99.50000000000000000, -24.13374913903897223 ) ) ;
#9458 = DIRECTION ( 'NONE',  ( 0.000000000000000000, 0.000000000000000000, 1.000000000000000000 ) ) ;
#9459 = EDGE_CURVE ( 'NONE', #5889, #5894, #3474, .T. ) ;
#9460 = CARTESIAN_POINT ( 'NONE',  ( -2.499999999999999556, -1.706249998770965615, 1.443375672974065882 ) ) ;
#9461 = ORIENTED_EDGE ( 'NONE', *, *, #914, .T. ) ;
#9462 = CARTESIAN_POINT ( 'NONE',  ( 3.948639947730041566, 99.99999999999998579, -21.07692942975820927 ) ) ;
#9463 = CARTESIAN_POINT ( 'NONE',  ( 1.653273178848927064E-15, 1.000000000000000000, -27.00000000000000355 ) ) ;
#9464 = CARTESIAN_POINT ( 'NONE',  ( 9.164845778125666698, 99.50000000000001421, 19.62003801130714820 ) ) ;
#9465 = CARTESIAN_POINT ( 'NONE',  ( 2.256430356250000546, -0.8531249993854829183, 1.302750673588579877 ) ) ;
#9466 = ORIENTED_EDGE ( 'NONE', *, *, #3951, .F. ) ;
#9467 = CARTESIAN_POINT ( 'NONE',  ( 3.044406660298407452, 99.50000000000000000, -23.15442635585071685 ) ) ;
#9468 = CARTESIAN_POINT ( 'NONE',  ( 9.445361748092775400, 100.0000000000000142, 19.75398588445988324 ) ) ;
#9469 = EDGE_CURVE ( 'NONE', #5423, #6706, #5139, .T. ) ;
#9470 = AXIS2_PLACEMENT_3D ( 'NONE', #275, #1162, #9954 ) ;
#9471 = CARTESIAN_POINT ( 'NONE',  ( -2.793760218496626182E-16, -25.00000000000000000, 2.062556682370379590 ) ) ;
#9472 = ORIENTED_EDGE ( 'NONE', *, *, #9027, .T. ) ;
#9473 = CARTESIAN_POINT ( 'NONE',  ( -14.97579057656165169, 99.50000000000001421, 16.56690896377573452 ) ) ;
#9474 = CARTESIAN_POINT ( 'NONE',  ( 27.43301270000000258, 4.349999998907525089, 0.000000000000000000 ) ) ;
#9475 = VERTEX_POINT ( 'NONE', #2740 ) ;
#9476 = CARTESIAN_POINT ( 'NONE',  ( 1.249999999999999334, -3.299999999999999378, -2.165063509461096825 ) ) ;
#9477 = AXIS2_PLACEMENT_3D ( 'NONE', #7391, #1794, #2688 ) ;
#9478 = CARTESIAN_POINT ( 'NONE',  ( 3.277744210708366079, 99.50000000000001421, -23.71256836663369327 ) ) ;
#9479 = CARTESIAN_POINT ( 'NONE',  ( 1.128215178125001161, -3.703124999385482230, 1.954126010382870815 ) ) ;
#9480 = EDGE_CURVE ( 'NONE', #4830, #1392, #232, .T. ) ;
#9481 = CARTESIAN_POINT ( 'NONE',  ( -16.87593989452418697, 99.49999999999998579, 15.58794934546231126 ) ) ;
#9482 = CARTESIAN_POINT ( 'NONE',  ( -19.39806930854667755, 3.849999998907525089, -19.39806930854668110 ) ) ;
#9483 = UNCERTAINTY_MEASURE_WITH_UNIT (LENGTH_MEASURE( 1.000000000000000082E-05 ), #10146, 'distance_accuracy_value', 'NONE');
#9484 = ADVANCED_FACE ( 'NONE', ( #972 ), #2918, .T. ) ;
#9485 = CARTESIAN_POINT ( 'NONE',  ( 4.909381318607588973, 99.50000000000000000, -23.54377677363417121 ) ) ;
#9486 = CARTESIAN_POINT ( 'NONE',  ( 3.428794695218988053, 100.0000000000000142, -24.07607503615978572 ) ) ;
#9487 = CARTESIAN_POINT ( 'NONE',  ( 2.843562173796539749, 99.50000000000001421, -21.91597968833000110 ) ) ;
#9488 = CARTESIAN_POINT ( 'NONE',  ( -22.08823018108446234, 100.0000000000000000, -9.406177930363766038 ) ) ;
#9489 = VECTOR ( 'NONE', #5596, 1000.000000000000114 ) ;
#9490 = CARTESIAN_POINT ( 'NONE',  ( -2.256430356250000102, -4.678124999385483207, -1.302750673588580321 ) ) ;
#9491 = CARTESIAN_POINT ( 'NONE',  ( 4.358720771404392735, 99.50000000000000000, -21.20742720589606378 ) ) ;
#9492 = CARTESIAN_POINT ( 'NONE',  ( -1.595409442497313560E-16, -2.503124999385482496, -2.605501347177161087 ) ) ;
#9493 = CARTESIAN_POINT ( 'NONE',  ( -11.36312591709335962, 0.5999999989075250895, -27.43301270000000258 ) ) ;
#9494 =( NAMED_UNIT ( * ) SI_UNIT ( $, .STERADIAN. ) SOLID_ANGLE_UNIT ( ) );
#9495 = VECTOR ( 'NONE', #10000, 1000.000000000000114 ) ;
#9496 = CARTESIAN_POINT ( 'NONE',  ( 0.6698729810778063509, -2.776346188203299814, -2.500000000000000000 ) ) ;
#9497 = CARTESIAN_POINT ( 'NONE',  ( -27.00000000000000355, 2.750000000000000888, -11.18376618407357093 ) ) ;
#9498 = CARTESIAN_POINT ( 'NONE',  ( 9.404665101723468368, 99.50000000000000000, 20.17141824467128686 ) ) ;
#9499 = AXIS2_PLACEMENT_3D ( 'NONE', #4545, #2081, #6739 ) ;
#9500 = ORIENTED_EDGE ( 'NONE', *, *, #7604, .T. ) ;
#9501 = CARTESIAN_POINT ( 'NONE',  ( -16.36254897777738648, 99.99999999999995737, 15.39785597259249172 ) ) ;
#9502 = CARTESIAN_POINT ( 'NONE',  ( 8.132491713109027742, 100.0000000000000142, 21.08089001807756446 ) ) ;
#9503 = CARTESIAN_POINT ( 'NONE',  ( 2.256430356250000102, -3.628124999385482496, -2.763330213280484622E-16 ) ) ;
#9504 = ORIENTED_EDGE ( 'NONE', *, *, #3753, .T. ) ;
#9505 = CARTESIAN_POINT ( 'NONE',  ( 11.36312591709336139, 2.799999998907524823, -27.43301270000000258 ) ) ;
#9506 = CARTESIAN_POINT ( 'NONE',  ( 3.409892249890944527, 99.50000000000000000, -24.50637943905448779 ) ) ;
#9507 = CONICAL_SURFACE ( 'NONE', #8985, 20.00000000000000000, 0.1745329251994333364 ) ;
#9508 = CARTESIAN_POINT ( 'NONE',  ( -1.128215178124998497, -1.528124999385482852, 1.954126010382872147 ) ) ;
#9509 = DIRECTION ( 'NONE',  ( 0.000000000000000000, 0.000000000000000000, -1.000000000000000000 ) ) ;
#9510 = CARTESIAN_POINT ( 'NONE',  ( -2.256430356250000102, -0.2531249993854829405, 0.000000000000000000 ) ) ;
#9511 = AXIS2_PLACEMENT_3D ( 'NONE', #4192, #9943, #9057 ) ;
#9512 = CARTESIAN_POINT ( 'NONE',  ( 2.500000000000000000, -2.831249998770965615, -1.443375672974064994 ) ) ;
#9513 = CARTESIAN_POINT ( 'NONE',  ( 4.433602057339688152, 100.0000000000000000, -21.25644978738549540 ) ) ;
#9514 = DIRECTION ( 'NONE',  ( 0.000000000000000000, 1.000000000000000000, 0.000000000000000000 ) ) ;
#9515 = CARTESIAN_POINT ( 'NONE',  ( 7.500000000000000000, 104.5000000000000142, 1.000000000000000222 ) ) ;
#9516 = CARTESIAN_POINT ( 'NONE',  ( 1.128215178125001161, -1.790624999385482807, 1.954126010382870815 ) ) ;
#9517 = B_SPLINE_CURVE_WITH_KNOTS ( 'NONE', 3,
 ( #8820, #7090, #8035, #6412, #131, #10295, #868, #9602, #9651, #3320, #2434, #5532, #7142, #4058, #2489, #1695, #4892, #917, #5868 ),
 .UNSPECIFIED., .F., .F.,
 ( 4, 1, 1, 1, 1, 1, 1, 1, 1, 1, 1, 1, 1, 1, 1, 1, 4 ),
 ( 0.000000000000000000, 0.06442465027149940626, 0.1272622498775801414, 0.1890519169419207224, 0.2498421757728049863, 0.3110425729590077792, 0.3720985300252119266, 0.4351465435385043490, 0.5001170788027262670, 0.5644817420234762295, 0.6276143074669133792, 0.6889588046791949028, 0.7501592018653976401, 0.8106582772613761811, 0.8724479443257179279, 0.9351683423010851426, 1.000000000000000000 ),
 .UNSPECIFIED. ) ;
#9518 = EDGE_CURVE ( 'NONE', #5650, #1313, #3523, .T. ) ;
#9519 = ORIENTED_EDGE ( 'NONE', *, *, #6569, .F. ) ;
#9520 = CARTESIAN_POINT ( 'NONE',  ( 9.877377282685029372E-16, -1.237499999999999600, 2.500000000000000000 ) ) ;
#9521 = CARTESIAN_POINT ( 'NONE',  ( 3.058419780146050648, 99.50000000000000000, -23.12871267107006545 ) ) ;
#9522 = CARTESIAN_POINT ( 'NONE',  ( -1.250000000000000222, -3.618749998770965259, -2.165063509461096825 ) ) ;
#9523 = CARTESIAN_POINT ( 'NONE',  ( -16.18965924272485779, 99.49999999999998579, 15.26525457555968224 ) ) ;
#9524 = CARTESIAN_POINT ( 'NONE',  ( 27.43301270000000258, 4.399999998907524912, -11.36312591709336139 ) ) ;
#9525 = EDGE_LOOP ( 'NONE', ( #9571, #6051, #4663, #6276 ) ) ;
#9526 = CARTESIAN_POINT ( 'NONE',  ( 2.500000000000000444, -4.312499999999999112, 1.443375672974063439 ) ) ;
#9527 = EDGE_CURVE ( 'NONE', #7809, #4040, #8338, .T. ) ;
#9528 = EDGE_CURVE ( 'NONE', #7541, #3111, #9707, .T. ) ;
#9529 = CARTESIAN_POINT ( 'NONE',  ( -20.89948324804827706, 100.0000000000000142, -10.26098411820691858 ) ) ;
#9530 = CARTESIAN_POINT ( 'NONE',  ( -2.256430356249999214, -4.265624999385482674, 1.302750673588581876 ) ) ;
#9531 = DIRECTION ( 'NONE',  ( 1.000000000000000000, 0.000000000000000000, 0.000000000000000000 ) ) ;
#9532 = CARTESIAN_POINT ( 'NONE',  ( -11.18376618407358336, 1.949999997815050401, 26.99999999999999645 ) ) ;
#9533 = FACE_OUTER_BOUND ( 'NONE', #637, .T. ) ;
#9534 = CARTESIAN_POINT ( 'NONE',  ( 3.535161742238301041, 100.0000000000000142, -24.18247714022527006 ) ) ;
#9535 = CARTESIAN_POINT ( 'NONE',  ( 3.611424427577684781, 99.50000000000001421, -21.45475674085064099 ) ) ;
#9536 = PRODUCT_DEFINITION_SHAPE ( 'NONE', 'NONE',  #1142 ) ;
#9537 = CARTESIAN_POINT ( 'NONE',  ( 27.00000000000000355, 4.000000000000000000, 0.000000000000000000 ) ) ;
#9538 = CARTESIAN_POINT ( 'NONE',  ( -2.256430356250000102, -4.190624999385482496, 0.000000000000000000 ) ) ;
#9539 = CARTESIAN_POINT ( 'NONE',  ( 4.280752963211088336, 99.99999999999997158, -21.16602454745684270 ) ) ;
#9540 = ORIENTED_EDGE ( 'NONE', *, *, #4405, .T. ) ;
#9541 = CARTESIAN_POINT ( 'NONE',  ( -2.256430356249999214, -3.253124999385482941, 1.302750673588581876 ) ) ;
#9542 = CARTESIAN_POINT ( 'NONE',  ( 27.43301270000000258, 0.3999999989075252449, -11.36312591709336139 ) ) ;
#9543 = CARTESIAN_POINT ( 'NONE',  ( 0.000000000000000000, 97.00000000000000000, 0.000000000000000000 ) ) ;
#9544 = CARTESIAN_POINT ( 'NONE',  ( 27.43301270000000258, 0.2999999989075253226, -11.36312591709336139 ) ) ;
#9545 = CARTESIAN_POINT ( 'NONE',  ( 3.028692941384139026, 100.0000000000000142, -22.52214499033115302 ) ) ;
#9546 = VECTOR ( 'NONE', #5799, 1000.000000000000000 ) ;
#9547 = CARTESIAN_POINT ( 'NONE',  ( 0.6698729810778112359, -3.282596189432334111, -2.499999999999996447 ) ) ;
#9548 = CARTESIAN_POINT ( 'NONE',  ( -15.62070810370258833, 99.50000000000000000, 16.62245103965875970 ) ) ;
#9549 = ORIENTED_EDGE ( 'NONE', *, *, #3419, .F. ) ;
#9550 = CARTESIAN_POINT ( 'NONE',  ( 1.128215178124999607, -4.903124999385481964, -1.954126010382871259 ) ) ;
#9551 = ORIENTED_EDGE ( 'NONE', *, *, #9811, .F. ) ;
#9552 = CARTESIAN_POINT ( 'NONE',  ( 11.36312591709336850, 1.699999998907525400, 27.43301269999999903 ) ) ;
#9553 = CARTESIAN_POINT ( 'NONE',  ( 3.350143586568126164, 99.50000000000001421, -24.46212657588250394 ) ) ;
#9554 = ADVANCED_FACE ( 'NONE', ( #8926 ), #3962, .F. ) ;
#9555 = CARTESIAN_POINT ( 'NONE',  ( -22.43115009631934953, 99.50000000000001421, -11.08196351649073819 ) ) ;
#9556 = CARTESIAN_POINT ( 'NONE',  ( -1.595409442497313560E-16, -3.515624999385482674, -2.605501347177161087 ) ) ;
#9557 = CARTESIAN_POINT ( 'NONE',  ( -27.00000000000000355, 1.799999997815050490, -3.306546357697854128E-15 ) ) ;
#9558 = CARTESIAN_POINT ( 'NONE',  ( -16.81182640597031508, 99.50000000000000000, 16.36129326314865295 ) ) ;
#9559 = CARTESIAN_POINT ( 'NONE',  ( 0.000000000000000000, 70.00000000000000000, 0.000000000000000000 ) ) ;
#9560 = CARTESIAN_POINT ( 'NONE',  ( 2.500000000000000000, -3.318749998770965437, -3.061616997868383141E-16 ) ) ;
#9561 = VERTEX_POINT ( 'NONE', #9175 ) ;
#9562 = CARTESIAN_POINT ( 'NONE',  ( 10.85214315541671759, 99.50000000000000000, 22.51047735782115211 ) ) ;
#9563 = DIRECTION ( 'NONE',  ( -0.7071067811865474617, -0.000000000000000000, 0.7071067811865476838 ) ) ;
#9564 = DIRECTION ( 'NONE',  ( 0.000000000000000000, 0.000000000000000000, -1.000000000000000000 ) ) ;
#9565 = CARTESIAN_POINT ( 'NONE',  ( 2.256430356250000546, -3.103124999385482585, 1.302750673588579877 ) ) ;
#9566 = ORIENTED_EDGE ( 'NONE', *, *, #121, .T. ) ;
#9567 = CARTESIAN_POINT ( 'NONE',  ( 2.927917759182871560, 99.49999999999997158, -23.69257214368879261 ) ) ;
#9568 = CARTESIAN_POINT ( 'NONE',  ( -7.500000000000000000, 104.5000000000000142, 1.000000000000000222 ) ) ;
#9569 = DIRECTION ( 'NONE',  ( -0.000000000000000000, 1.000000000000000000, -0.000000000000000000 ) ) ;
#9570 = CARTESIAN_POINT ( 'NONE',  ( 27.43301270000000258, 3.599999998907525534, -11.36312591709336139 ) ) ;
#9571 = ORIENTED_EDGE ( 'NONE', *, *, #3890, .F. ) ;
#9572 = CARTESIAN_POINT ( 'NONE',  ( -2.499999999999999556, -3.562500000000000444, 1.443375672974065882 ) ) ;
#9573 = CARTESIAN_POINT ( 'NONE',  ( -20.93486371557392545, 99.99999999999998579, -10.61231311368802466 ) ) ;
#9574 = CARTESIAN_POINT ( 'NONE',  ( -2.256430356249999214, -4.715624999385481964, 1.302750673588581876 ) ) ;
#9575 = CARTESIAN_POINT ( 'NONE',  ( -20.70854316912038229, 100.0000000000000142, -10.95957977981033515 ) ) ;
#9576 = CARTESIAN_POINT ( 'NONE',  ( 19.39806930854668110, 4.449999998907525622, -19.39806930854668110 ) ) ;
#9577 = AXIS2_PLACEMENT_3D ( 'NONE', #1256, #9886, #6850 ) ;
#9578 = CARTESIAN_POINT ( 'NONE',  ( -15.11748654497029953, 99.99999999999995737, 15.76872032455190897 ) ) ;
#9579 = CARTESIAN_POINT ( 'NONE',  ( 3.349514647153394975, 99.99999999999998579, -23.95461210612682024 ) ) ;
#9580 = CARTESIAN_POINT ( 'NONE',  ( 3.739209042966563867, 100.0000000000000000, -21.42288334414699236 ) ) ;
#9581 = ADVANCED_FACE ( 'NONE', ( #5246, #7825 ), #9394, .T. ) ;
#9582 = DIRECTION ( 'NONE',  ( -1.000000000000000000, -1.224646799147352961E-16, 0.000000000000000000 ) ) ;
#9583 = CARTESIAN_POINT ( 'NONE',  ( 2.256430356250000102, -3.065624999385482496, -2.763330213280484622E-16 ) ) ;
#9584 = CARTESIAN_POINT ( 'NONE',  ( 0.000000000000000000, -25.00000000000000000, -0.4999999999999953371 ) ) ;
#9585 = CARTESIAN_POINT ( 'NONE',  ( 1.128215178125001161, -1.340624999385482852, 1.954126010382870815 ) ) ;
#9586 = CARTESIAN_POINT ( 'NONE',  ( -27.43301270000000258, 0.6999999989075252893, -11.36312591709336317 ) ) ;
#9587 = FILL_AREA_STYLE_COLOUR ( '', #6730 ) ;
#9588 = LINE ( 'NONE', #7915, #8936 ) ;
#9589 =( GEOMETRIC_REPRESENTATION_CONTEXT ( 3 ) GLOBAL_UNCERTAINTY_ASSIGNED_CONTEXT ( ( #8010 ) ) GLOBAL_UNIT_ASSIGNED_CONTEXT ( ( #1005, #2675, #7481 ) ) REPRESENTATION_CONTEXT ( 'NONE', 'WORKASPACE' ) );
#9590 = CARTESIAN_POINT ( 'NONE',  ( -11.18376618407356560, 3.450000000000000178, -27.00000000000000355 ) ) ;
#9591 = PLANE ( 'NONE',  #877 ) ;
#9592 = CARTESIAN_POINT ( 'NONE',  ( -16.37547766376588854, 99.99999999999995737, 16.41943072543956816 ) ) ;
#9593 = CARTESIAN_POINT ( 'NONE',  ( 8.540544597724410991, 99.50000000000000000, 19.98924338346217766 ) ) ;
#9594 = ORIENTED_EDGE ( 'NONE', *, *, #7948, .T. ) ;
#9595 =( BOUNDED_CURVE ( )  B_SPLINE_CURVE ( 2, ( #1967, #1192, #5850, #7322, #6538 ),
 .UNSPECIFIED., .F., .F. ) 
 B_SPLINE_CURVE_WITH_KNOTS ( ( 3, 2, 3 ),
 ( 0.000000000000000000, 0.01388888888888888985, 0.02083333333333333565 ),
 .UNSPECIFIED. ) 
 CURVE ( )  GEOMETRIC_REPRESENTATION_ITEM ( )  RATIONAL_B_SPLINE_CURVE ( ( 1.000000000000000000, 0.8660254037844387076, 1.000000000000000000, 0.9330127018922192983, 0.9330127018922194093 ) ) 
 REPRESENTATION_ITEM ( '' )  );
#9596 = CARTESIAN_POINT ( 'NONE',  ( 4.786228327491941173E-16, -4.640624999385482674, 2.605501347177161087 ) ) ;
#9597 = ORIENTED_EDGE ( 'NONE', *, *, #5985, .F. ) ;
#9598 = CARTESIAN_POINT ( 'NONE',  ( 27.43301270000000258, 1.899999998907525134, -11.36312591709336139 ) ) ;
#9599 = CARTESIAN_POINT ( 'NONE',  ( 2.950788281418828429, 99.50000000000001421, -23.82341910423825837 ) ) ;
#9600 = DIRECTION ( 'NONE',  ( 0.3924386850477849520, 0.000000000000000000, 0.9197781680807419757 ) ) ;
#9601 = CARTESIAN_POINT ( 'NONE',  ( 1.128215178124999607, -4.903124999385481964, -1.954126010382871259 ) ) ;
#9602 = CARTESIAN_POINT ( 'NONE',  ( -16.56356094049941419, 99.99999999999997158, 15.77213757552179629 ) ) ;
#9603 = CARTESIAN_POINT ( 'NONE',  ( -22.67573144110267336, 100.0000000000000142, -10.14737752305977381 ) ) ;
#9604 = DIRECTION ( 'NONE',  ( -0.000000000000000000, 0.000000000000000000, -1.000000000000000000 ) ) ;
#9605 = EDGE_CURVE ( 'NONE', #6035, #4027, #9127, .T. ) ;
#9606 = EDGE_CURVE ( 'NONE', #9074, #7561, #2847, .T. ) ;
#9607 = CARTESIAN_POINT ( 'NONE',  ( -1.250000000000000222, -1.368749998770965925, -2.165063509461096825 ) ) ;
#9608 = ORIENTED_EDGE ( 'NONE', *, *, #8746, .F. ) ;
#9609 = CARTESIAN_POINT ( 'NONE',  ( 4.386516977709190357, 100.0000000000000568, -24.31220192127581825 ) ) ;
#9610 = CARTESIAN_POINT ( 'NONE',  ( -20.63666786535793207, 99.49999999999998579, -10.16306733409737717 ) ) ;
#9611 = CARTESIAN_POINT ( 'NONE',  ( -21.72555844818415594, 99.50000000000001421, -11.09629251537910655 ) ) ;
#9612 = CARTESIAN_POINT ( 'NONE',  ( -2.256430356249999658, -5.114265559567681585, -0.8212734853698877568 ) ) ;
#9613 = PRODUCT_DEFINITION_SHAPE ( 'NONE', 'NONE',  #10368 ) ;
#9614 = ORIENTED_EDGE ( 'NONE', *, *, #7105, .T. ) ;
#9615 = CARTESIAN_POINT ( 'NONE',  ( -22.17094027205346052, 100.0000000000000142, -9.884352203306939089 ) ) ;
#9616 = VERTEX_POINT ( 'NONE', #436 ) ;
#9617 = VECTOR ( 'NONE', #296, 1000.000000000000000 ) ;
#9618 = SURFACE_SIDE_STYLE ('',( #4750 ) ) ;
#9619 = CARTESIAN_POINT ( 'NONE',  ( -21.96365545856212265, 99.50000000000001421, -9.726658277667754149 ) ) ;
#9620 = CARTESIAN_POINT ( 'NONE',  ( 27.00000000000000355, 3.049999997815050268, -11.18376618407356915 ) ) ;
#9621 = CARTESIAN_POINT ( 'NONE',  ( 19.39806930854668110, 5.249999998907525445, -19.39806930854668110 ) ) ;
#9622 = ORIENTED_EDGE ( 'NONE', *, *, #7643, .T. ) ;
#9623 =( LENGTH_UNIT ( ) NAMED_UNIT ( * ) SI_UNIT ( .MILLI., .METRE. ) );
#9624 = VECTOR ( 'NONE', #5121, 1000.000000000000000 ) ;
#9625 = CARTESIAN_POINT ( 'NONE',  ( 3.341734429721257005, 100.0000000000000000, -22.34498040423979148 ) ) ;
#9626 = CARTESIAN_POINT ( 'NONE',  ( 2.256430356250000102, -4.528124999385481964, -2.763330213280484622E-16 ) ) ;
#9627 = CARTESIAN_POINT ( 'NONE',  ( -20.89145576992255116, 99.49999999999997158, -10.33073932272468198 ) ) ;
#9628 = CARTESIAN_POINT ( 'NONE',  ( 27.00000000000000355, 2.199999997815050623, 0.000000000000000000 ) ) ;
#9629 = CARTESIAN_POINT ( 'NONE',  ( -4.357666448243394824E-15, -2.137500000000000178, 2.500000000000000000 ) ) ;
#9630 = CARTESIAN_POINT ( 'NONE',  ( 3.282077632710153292, 99.50000000000000000, -23.74569985055724786 ) ) ;
#9631 = CARTESIAN_POINT ( 'NONE',  ( 3.739209042966563867, 99.50000000000000000, -21.42288334414699236 ) ) ;
#9632 = LINE ( 'NONE', #2466, #4797 ) ;
#9633 = CARTESIAN_POINT ( 'NONE',  ( 2.256430356249999658, -3.028124999385482852, -1.302750673588581432 ) ) ;
#9634 = CARTESIAN_POINT ( 'NONE',  ( 9.902568905804752575, 99.99999999999998579, 20.48863403721516363 ) ) ;
#9635 = EDGE_LOOP ( 'NONE', ( #2868, #819, #4574, #1835 ) ) ;
#9636 = CARTESIAN_POINT ( 'NONE',  ( -1.595409442497313560E-16, -2.053124999385482763, -2.605501347177161087 ) ) ;
#9637 = CARTESIAN_POINT ( 'NONE',  ( 11.36312591709336139, 0.4999999989075251672, -27.43301270000000258 ) ) ;
#9638 = SURFACE_STYLE_USAGE ( .BOTH. , #5564 ) ;
#9639 = CARTESIAN_POINT ( 'NONE',  ( -7.500000000000000888, 105.0000000000000142, 3.000000000000000000 ) ) ;
#9640 = EDGE_CURVE ( 'NONE', #2167, #3761, #7598, .T. ) ;
#9641 = CARTESIAN_POINT ( 'NONE',  ( 26.99999999999999645, 4.750000000000001776, 11.18376618407358691 ) ) ;
#9642 = CARTESIAN_POINT ( 'NONE',  ( -21.13504512532655610, 100.0000000000000000, -11.31853095674525100 ) ) ;
#9643 = AXIS2_PLACEMENT_3D ( 'NONE', #6856, #2209, #5355 ) ;
#9644 = CARTESIAN_POINT ( 'NONE',  ( -21.18296228862668329, 100.0000000000000000, -10.95406920104765724 ) ) ;
#9645 = CARTESIAN_POINT ( 'NONE',  ( 24.91446314102564230, 99.50000000000000000, -1.581029647435897578 ) ) ;
#9646 = ORIENTED_EDGE ( 'NONE', *, *, #8261, .T. ) ;
#9647 = AXIS2_PLACEMENT_3D ( 'NONE', #5804, #1764, #7364 ) ;
#9648 = CARTESIAN_POINT ( 'NONE',  ( 1.679787559701184688E-15, 1.249999998907525223, -27.43301270000000258 ) ) ;
#9649 = CYLINDRICAL_SURFACE ( 'NONE', #3386, 27.00000000000000355 ) ;
#9650 = CARTESIAN_POINT ( 'NONE',  ( -1.128215178124998497, -3.328124999385482230, 1.954126010382872147 ) ) ;
#9651 = CARTESIAN_POINT ( 'NONE',  ( -16.57330815294036697, 100.0000000000000142, 15.84440382193293217 ) ) ;
#9652 = EDGE_CURVE ( 'NONE', #1073, #3821, #1223, .T. ) ;
#9653 = CARTESIAN_POINT ( 'NONE',  ( -16.90147242988460263, 99.49999999999998579, 15.68472263728856753 ) ) ;
#9654 = CARTESIAN_POINT ( 'NONE',  ( 8.091962505948220752, 99.99999999999995737, 20.48385654212622242 ) ) ;
#9655 = VERTEX_POINT ( 'NONE', #493 ) ;
#9656 =( BOUNDED_CURVE ( )  B_SPLINE_CURVE ( 2, ( #2212, #9496, #10114, #5415, #2951, #6242, #2157, #5359, #7815 ),
 .UNSPECIFIED., .F., .T. ) 
 B_SPLINE_CURVE_WITH_KNOTS ( ( 3, 2, 2, 2, 3 ),
 ( 0.4375000000000000000, 0.4444444444444444198, 0.4583333333333333148, 0.4722222222222222099, 0.4791666666666666852 ),
 .UNSPECIFIED. ) 
 CURVE ( )  GEOMETRIC_REPRESENTATION_ITEM ( )  RATIONAL_B_SPLINE_CURVE ( ( 0.9330127018922194093, 0.9330127018922194093, 1.000000000000000000, 0.8660254037844387076, 1.000000000000000000, 0.8660254037844387076, 1.000000000000000000, 0.9330127018922190762, 0.9330127018922194093 ) ) 
 REPRESENTATION_ITEM ( '' )  );
#9657 = AXIS2_PLACEMENT_3D ( 'NONE', #466, #6842, #5396 ) ;
#9658 = CARTESIAN_POINT ( 'NONE',  ( 5.302876193624534821E-16, -3.881249998770965437, 2.886751345948128655 ) ) ;
#9659 = EDGE_LOOP ( 'NONE', ( #4275, #120, #4048, #4127 ) ) ;
#9660 = CARTESIAN_POINT ( 'NONE',  ( 4.584380863705032283, 99.50000000000001421, -24.21384527865288305 ) ) ;
#9661 = CARTESIAN_POINT ( 'NONE',  ( -15.32348647777738826, 99.50000000000000000, 15.39505148541300450 ) ) ;
#9662 = DIRECTION ( 'NONE',  ( 0.8660254037844393737, 0.4999999999999988898, 0.000000000000000000 ) ) ;
#9663 = CARTESIAN_POINT ( 'NONE',  ( -1.595409442497313560E-16, -4.753124999385481608, -2.605501347177161087 ) ) ;
#9664 = EDGE_CURVE ( 'NONE', #2104, #498, #5236, .T. ) ;
#9665 = ORIENTED_EDGE ( 'NONE', *, *, #874, .F. ) ;
#9666 = VECTOR ( 'NONE', #8596, 1000.000000000000000 ) ;
#9667 = EDGE_CURVE ( 'NONE', #7275, #7177, #4576, .T. ) ;
#9668 = CARTESIAN_POINT ( 'NONE',  ( 9.877377282685029372E-16, -2.081249998770965615, 2.500000000000000000 ) ) ;
#9669 = CARTESIAN_POINT ( 'NONE',  ( 19.09188309203678102, 2.899999997815050357, 19.09188309203678813 ) ) ;
#9670 = CARTESIAN_POINT ( 'NONE',  ( 9.404665101723468368, 100.0000000000000000, 20.17141824467128686 ) ) ;
#9671 = CARTESIAN_POINT ( 'NONE',  ( 4.472992770554171216, 99.49999999999998579, -21.83386288566719458 ) ) ;
#9672 = EDGE_CURVE ( 'NONE', #653, #7728, #10210, .T. ) ;
#9673 = CARTESIAN_POINT ( 'NONE',  ( 2.837666006185522782, 99.50000000000000000, -22.03040394835428373 ) ) ;
#9674 = CARTESIAN_POINT ( 'NONE',  ( -2.256430356250000102, -3.853124999385482585, 0.000000000000000000 ) ) ;
#9675 = VERTEX_POINT ( 'NONE', #1102 ) ;
#9676 = CARTESIAN_POINT ( 'NONE',  ( 4.100286767325537873, 100.0000000000000284, -22.51382885696750336 ) ) ;
#9677 = CARTESIAN_POINT ( 'NONE',  ( -11.36312591709337383, 4.899999998907526688, 27.43301269999999548 ) ) ;
#9678 = DIRECTION ( 'NONE',  ( 0.2499845035238856816, 0.000000000000000000, -0.9682498375925071565 ) ) ;
#9679 = CARTESIAN_POINT ( 'NONE',  ( 3.535161742238301041, 99.50000000000001421, -24.18247714022527006 ) ) ;
#9680 = CARTESIAN_POINT ( 'NONE',  ( 3.269123371500344710, 100.0000000000000142, -23.64665713169964434 ) ) ;
#9681 = CARTESIAN_POINT ( 'NONE',  ( -22.21668755910108928, 100.0000000000000426, -9.472979539922778969 ) ) ;
#9682 = CARTESIAN_POINT ( 'NONE',  ( -1.128215178125000273, -4.715624999385481964, -1.954126010382871259 ) ) ;
#9683 = CARTESIAN_POINT ( 'NONE',  ( 2.500000000000000000, -2.437500000000000000, -1.443375672974065438 ) ) ;
#9684 = PRESENTATION_LAYER_ASSIGNMENT (  '', '', ( #663 ) ) ;
#9685 = CARTESIAN_POINT ( 'NONE',  ( -1.128215178125000273, -3.815624999385482941, -1.954126010382871259 ) ) ;
#9686 =( LENGTH_UNIT ( ) NAMED_UNIT ( * ) SI_UNIT ( .MILLI., .METRE. ) );
#9687 = CARTESIAN_POINT ( 'NONE',  ( -16.60513711880302878, 99.50000000000000000, 15.15667007515659570 ) ) ;
#9688 = CARTESIAN_POINT ( 'NONE',  ( -11.36312591709337383, 0.7999999989075252671, 27.43301269999999548 ) ) ;
#9689 = CARTESIAN_POINT ( 'NONE',  ( 10.72103337977569204, 99.50000000000000000, 22.20268488987243316 ) ) ;
#9690 = DIRECTION ( 'NONE',  ( 0.000000000000000000, 1.000000000000000000, -0.000000000000000000 ) ) ;
#9691 = CARTESIAN_POINT ( 'NONE',  ( -20.91430522584054330, 99.50000000000001421, -10.19152558580213608 ) ) ;
#9692 = ORIENTED_EDGE ( 'NONE', *, *, #7602, .T. ) ;
#9693 = CARTESIAN_POINT ( 'NONE',  ( 1.249999999999999334, -5.043749998770965526, -2.165063509461096825 ) ) ;
#9694 = CARTESIAN_POINT ( 'NONE',  ( 19.39806930854668110, 5.149999998907524912, -19.39806930854668110 ) ) ;
#9695 = CARTESIAN_POINT ( 'NONE',  ( 0.000000000000000000, 75.00000000000001421, 0.000000000000000000 ) ) ;
#9696 = CARTESIAN_POINT ( 'NONE',  ( -19.09188309203678813, 1.099999997815050312, 19.09188309203678457 ) ) ;
#9697 = CARTESIAN_POINT ( 'NONE',  ( 2.256430356250000102, -4.078124999385482674, -2.763330213280484622E-16 ) ) ;
#9698 = CARTESIAN_POINT ( 'NONE',  ( -11.18376618407356737, 1.649999997815050579, -27.00000000000000355 ) ) ;
#9699 = B_SPLINE_CURVE_WITH_KNOTS ( 'NONE', 3,
 ( #8428, #4448, #4398, #6799, #8373, #6963, #2885, #7753, #6068, #9999, #3002, #1204, #1258, #421, #9205, #4502, #7694, #6233, #9318 ),
 .UNSPECIFIED., .F., .F.,
 ( 4, 1, 1, 1, 1, 1, 1, 1, 1, 1, 1, 1, 1, 1, 1, 1, 4 ),
 ( 0.000000000000000000, 0.07313710028058939550, 0.1429478298248799129, 0.2105045057187734658, 0.2751999312753631854, 0.3390602298032547868, 0.4018764873508149926, 0.4650016082884899093, 0.5281538368899733049, 0.5906348070863262079, 0.6510495490485337378, 0.7103018853965116230, 0.7674338915725752441, 0.8249350906448947862, 0.8823686014076175255, 0.9405824579944982444, 1.000000000000000000 ),
 .UNSPECIFIED. ) ;
#9700 = CARTESIAN_POINT ( 'NONE',  ( -16.60513711880302878, 99.50000000000000000, 15.15667007515659570 ) ) ;
#9701 = CARTESIAN_POINT ( 'NONE',  ( 8.132491713109025966, 100.0000000000000000, 21.08089001807756091 ) ) ;
#9702 = CARTESIAN_POINT ( 'NONE',  ( 2.500000000000000000, -5.081249998770965171, -1.443375672974064994 ) ) ;
#9703 = ORIENTED_EDGE ( 'NONE', *, *, #1009, .T. ) ;
#9704 = EDGE_CURVE ( 'NONE', #5989, #4002, #5385, .T. ) ;
#9705 = AXIS2_PLACEMENT_3D ( 'NONE', #9413, #3816, #2345 ) ;
#9706 = CARTESIAN_POINT ( 'NONE',  ( -22.35673484330673944, 99.50000000000001421, -10.41320610523044721 ) ) ;
#9707 = LINE ( 'NONE', #2545, #7300 ) ;
#9708 = CARTESIAN_POINT ( 'NONE',  ( -17.94007301623892658, 99.50000000000000000, 17.49000340848992607 ) ) ;
#9709 = CARTESIAN_POINT ( 'NONE',  ( -1.128215178125000273, -4.265624999385482674, -1.954126010382871259 ) ) ;
#9710 = ORIENTED_EDGE ( 'NONE', *, *, #966, .T. ) ;
#9711 = CARTESIAN_POINT ( 'NONE',  ( -15.31787750341841559, 99.50000000000001421, 16.43551622900274722 ) ) ;
#9712 = CARTESIAN_POINT ( 'NONE',  ( 0.000000000000000000, 97.00000000000000000, 0.000000000000000000 ) ) ;
#9713 = FACE_OUTER_BOUND ( 'NONE', #6981, .T. ) ;
#9714 = CARTESIAN_POINT ( 'NONE',  ( 8.684839681857363658, 100.0000000000000142, 19.94043386883836178 ) ) ;
#9715 = VERTEX_POINT ( 'NONE', #8175 ) ;
#9716 = VECTOR ( 'NONE', #8096, 1000.000000000000114 ) ;
#9717 = CARTESIAN_POINT ( 'NONE',  ( 3.845216150098881513, 99.50000000000000000, -21.40922359334548020 ) ) ;
#9718 = CARTESIAN_POINT ( 'NONE',  ( -20.61566945723384592, 99.50000000000000000, -10.83949095114527594 ) ) ;
#9719 = CARTESIAN_POINT ( 'NONE',  ( 19.09188309203678102, 1.299999997815050268, 19.09188309203678813 ) ) ;
#9720 = EDGE_CURVE ( 'NONE', #6902, #463, #4104, .T. ) ;
#9721 = CARTESIAN_POINT ( 'NONE',  ( -20.70854316912038229, 99.50000000000001421, -10.95957977981033515 ) ) ;
#9722 = CARTESIAN_POINT ( 'NONE',  ( 0.6698729810778075722, -4.761153809338632747, 2.499999999999999556 ) ) ;
#9723 = CARTESIAN_POINT ( 'NONE',  ( -15.91084591538827198, 99.50000000000001421, 16.65047278764667027 ) ) ;
#9724 = AXIS2_PLACEMENT_3D ( 'NONE', #994, #5905, #1094 ) ;
#9725 = EDGE_CURVE ( 'NONE', #570, #6922, #5127, .T. ) ;
#9726 = CARTESIAN_POINT ( 'NONE',  ( -22.11394672483139701, 100.0000000000000000, -10.91855052283267646 ) ) ;
#9727 = CYLINDRICAL_SURFACE ( 'NONE', #9647, 25.15000000000000213 ) ;
#9728 = VERTEX_POINT ( 'NONE', #5914 ) ;
#9729 = CARTESIAN_POINT ( 'NONE',  ( 2.256430356250000102, -4.865624999385482319, -2.763330213280484622E-16 ) ) ;
#9730 =( NAMED_UNIT ( * ) PLANE_ANGLE_UNIT ( ) SI_UNIT ( $, .RADIAN. ) );
#9731 = DIRECTION ( 'NONE',  ( -0.000000000000000000, 1.000000000000000000, -0.000000000000000000 ) ) ;
#9732 = CARTESIAN_POINT ( 'NONE',  ( -2.256430356249999214, -0.6656249993854828073, 1.302750673588581876 ) ) ;
#9733 = CARTESIAN_POINT ( 'NONE',  ( 11.18376618407356915, 4.150000000000000355, -27.00000000000000355 ) ) ;
#9734 = DIRECTION ( 'NONE',  ( 0.000000000000000000, 1.000000000000000000, 0.000000000000000000 ) ) ;
#9735 = LINE ( 'NONE', #3452, #5262 ) ;
#9736 = SHAPE_REPRESENTATION ( 'grease nipple', ( #5055 ), #7312 ) ;
#9737 = CARTESIAN_POINT ( 'NONE',  ( -19.75840245672548789, 99.50000000000000000, -8.735905494466331689 ) ) ;
#9738 = CARTESIAN_POINT ( 'NONE',  ( -21.28703419482447146, 99.99999999999994316, -11.01737971290317297 ) ) ;
#9739 = CARTESIAN_POINT ( 'NONE',  ( 1.653273178848927064E-15, 0.2000000000000000111, -27.00000000000000355 ) ) ;
#9740=STYLED_ITEM('',(#10394),#2806);
#9741 = DIRECTION ( 'NONE',  ( -0.3368610894541371747, 0.000000000000000000, 0.9415543565890243105 ) ) ;
#9742 = VECTOR ( 'NONE', #4527, 1000.000000000000000 ) ;
#9743 = CARTESIAN_POINT ( 'NONE',  ( -19.39806930854668465, 0.7499999989075251117, 19.39806930854667755 ) ) ;
#9744 = DIRECTION ( 'NONE',  ( 1.000000000000000000, 0.000000000000000000, 0.000000000000000000 ) ) ;
#9745 = CARTESIAN_POINT ( 'NONE',  ( -1.128215178124998497, -2.878124999385482496, 1.954126010382872147 ) ) ;
#9746 = CARTESIAN_POINT ( 'NONE',  ( -22.69331084068295112, 99.49999999999998579, -10.43328931840349050 ) ) ;
#9747 = CARTESIAN_POINT ( 'NONE',  ( -22.67341330918043951, 100.0000000000000000, -10.57563951594260665 ) ) ;
#9748 = CARTESIAN_POINT ( 'NONE',  ( 26.99999999999999645, 5.349999997815049646, 11.18376618407358691 ) ) ;
#9749 = MECHANICAL_DESIGN_GEOMETRIC_PRESENTATION_REPRESENTATION (  '', ( #903 ), #8921 ) ;
#9750 = CARTESIAN_POINT ( 'NONE',  ( -1.767625397874844694E-16, -4.106249998770965526, -2.886751345948128655 ) ) ;
#9751 = ORIENTED_EDGE ( 'NONE', *, *, #2957, .T. ) ;
#9752 = ORIENTED_EDGE ( 'NONE', *, *, #839, .T. ) ;
#9753 = CARTESIAN_POINT ( 'NONE',  ( -22.34945848979098670, 99.50000000000002842, -10.27225542379191481 ) ) ;
#9754 = CARTESIAN_POINT ( 'NONE',  ( 3.717146347979291665, 99.99999999999997158, -21.42716062222556417 ) ) ;
#9755 = DIRECTION ( 'NONE',  ( 0.8579654788304353907, 0.000000000000000000, -0.5137073458062109133 ) ) ;
#9756 = CARTESIAN_POINT ( 'NONE',  ( -2.256430356250000102, -3.290624999385482585, 0.000000000000000000 ) ) ;
#9757 = ADVANCED_FACE ( 'NONE', ( #7427 ), #9111, .T. ) ;
#9758 = DIRECTION ( 'NONE',  ( -0.000000000000000000, 1.000000000000000000, -0.000000000000000000 ) ) ;
#9759 = LINE ( 'NONE', #3333, #6157 ) ;
#9760 = CARTESIAN_POINT ( 'NONE',  ( -4.959819536546781389E-15, 2.799999997815050268, 27.00000000000000355 ) ) ;
#9761 = CARTESIAN_POINT ( 'NONE',  ( 3.124251205490514494, 99.50000000000000000, -23.02140944421609703 ) ) ;
#9762 = CARTESIAN_POINT ( 'NONE',  ( -2.500000000000000000, -4.500000000000000000, 0.000000000000000000 ) ) ;
#9763 = FACE_OUTER_BOUND ( 'NONE', #7342, .T. ) ;
#9764 = CIRCLE ( 'NONE', #766, 22.50000000000000355 ) ;
#9765 = EDGE_CURVE ( 'NONE', #10197, #4536, #3359, .T. ) ;
#9766 = ORIENTED_EDGE ( 'NONE', *, *, #1596, .T. ) ;
#9767 = CARTESIAN_POINT ( 'NONE',  ( 9.820792995160308791, 99.50000000000000000, 20.21220011423140761 ) ) ;
#9768 = CARTESIAN_POINT ( 'NONE',  ( -27.00000000000001421, 2.649999997815050357, 11.18376618407356382 ) ) ;
#9769 = PLANE ( 'NONE',  #7695 ) ;
#9770 = CARTESIAN_POINT ( 'NONE',  ( -21.31369174262763622, 99.99999999999997158, -9.710155485040722567 ) ) ;
#9771 = DIRECTION ( 'NONE',  ( 0.000000000000000000, 0.000000000000000000, -1.000000000000000000 ) ) ;
#9772 = CARTESIAN_POINT ( 'NONE',  ( -21.37606745505193473, 100.0000000000000284, -11.05925878703054011 ) ) ;
#9773 = CARTESIAN_POINT ( 'NONE',  ( 0.6698729810778025762, -4.817403810567666866, 2.500000000000002665 ) ) ;
#9774 = AXIS2_PLACEMENT_3D ( 'NONE', #10305, #4749, #3138 ) ;
#9775 = ORIENTED_EDGE ( 'NONE', *, *, #10245, .F. ) ;
#9776 = CARTESIAN_POINT ( 'NONE',  ( -0.7001057366827120321, -5.193520385083734148, -2.676043109347841398 ) ) ;
#9777 = EDGE_CURVE ( 'NONE', #5851, #9561, #859, .T. ) ;
#9778 = CARTESIAN_POINT ( 'NONE',  ( 3.306546357697853733E-15, 0.000000000000000000, 27.00000000000000000 ) ) ;
#9779 = CARTESIAN_POINT ( 'NONE',  ( 2.924645347134957163, 99.50000000000001421, -23.60918035669702064 ) ) ;
#9780 = CARTESIAN_POINT ( 'NONE',  ( 1.679787559701184688E-15, 2.849999998907525534, -27.43301270000000258 ) ) ;
#9781 = CARTESIAN_POINT ( 'NONE',  ( 27.43301270000000258, 0.3999999989075252449, -11.36312591709336139 ) ) ;
#9782 = DIRECTION ( 'NONE',  ( 0.000000000000000000, 0.000000000000000000, -1.000000000000000000 ) ) ;
#9783 = CARTESIAN_POINT ( 'NONE',  ( 0.000000000000000000, 85.00000000000000000, 0.000000000000000000 ) ) ;
#9784 = CARTESIAN_POINT ( 'NONE',  ( -21.03403678956047074, 99.99999999999998579, -10.80451401317004922 ) ) ;
#9785 = EDGE_CURVE ( 'NONE', #1485, #7672, #7641, .T. ) ;
#9786 = EDGE_LOOP ( 'NONE', ( #2499, #4269, #1449, #5215 ) ) ;
#9787 = CARTESIAN_POINT ( 'NONE',  ( -22.05573893622344173, 99.50000000000000000, -9.391591294897233766 ) ) ;
#9788 = CARTESIAN_POINT ( 'NONE',  ( 3.238942592553923472, 100.0000000000000142, -24.36085717291697250 ) ) ;
#9789 = CARTESIAN_POINT ( 'NONE',  ( 9.431378708427812896, 99.49999999999998579, 21.34379071326255684 ) ) ;
#9790 = CARTESIAN_POINT ( 'NONE',  ( -21.29537297865864431, 100.0000000000000000, -11.39144590536739976 ) ) ;
#9791 = CARTESIAN_POINT ( 'NONE',  ( 19.09188309203678102, 4.700000000000000178, 19.09188309203678813 ) ) ;
#9792 = FACE_OUTER_BOUND ( 'NONE', #9635, .T. ) ;
#9793 = CARTESIAN_POINT ( 'NONE',  ( -22.08823018108446234, 99.50000000000000000, -9.406177930363766038 ) ) ;
#9794 = VECTOR ( 'NONE', #4632, 1000.000000000000000 ) ;
#9795 = CARTESIAN_POINT ( 'NONE',  ( 8.187169943530866689, 99.99999999999998579, 20.27434297626003712 ) ) ;
#9796 = ORIENTED_EDGE ( 'NONE', *, *, #9725, .F. ) ;
#9797 = VERTEX_POINT ( 'NONE', #8488 ) ;
#9798 = CARTESIAN_POINT ( 'NONE',  ( -1.767625397874844694E-16, -5.006249998770964993, -2.886751345948128655 ) ) ;
#9799 = ORIENTED_EDGE ( 'NONE', *, *, #7879, .F. ) ;
#9800 = EDGE_LOOP ( 'NONE', ( #3145, #8272, #2349, #3736 ) ) ;
#9801 = AXIS2_PLACEMENT_3D ( 'NONE', #4331, #3493, #4051 ) ;
#9802 = DIRECTION ( 'NONE',  ( 0.000000000000000000, 0.000000000000000000, -1.000000000000000000 ) ) ;
#9803 = DIRECTION ( 'NONE',  ( 0.9789429660840185399, 0.000000000000000000, -0.2041339490496966447 ) ) ;
#9804 = CARTESIAN_POINT ( 'NONE',  ( 21.79306891025641235, 100.0000000000000000, -1.065004006410256387 ) ) ;
#9805 = CARTESIAN_POINT ( 'NONE',  ( 9.248677610544923766, 99.50000000000000000, 22.83089001807756446 ) ) ;
#9806 = PRODUCT_DEFINITION_FORMATION_WITH_SPECIFIED_SOURCE ( 'ANY', '', #8779, .NOT_KNOWN. ) ;
#9807 = LINE ( 'NONE', #930, #6621 ) ;
#9808 = DIRECTION ( 'NONE',  ( -0.000000000000000000, 1.000000000000000000, -0.000000000000000000 ) ) ;
#9809 = CARTESIAN_POINT ( 'NONE',  ( -3.000000000000000888, -15.00000000000000000, 1.732050807568878303 ) ) ;
#9810 = ORIENTED_EDGE ( 'NONE', *, *, #9640, .F. ) ;
#9811 = EDGE_CURVE ( 'NONE', #2830, #5851, #10145, .T. ) ;
#9812 = CARTESIAN_POINT ( 'NONE',  ( 4.446585460023182890, 99.50000000000002842, -21.79057454014859019 ) ) ;
#9813 = CARTESIAN_POINT ( 'NONE',  ( 1.679787559701184688E-15, 5.249999998907525445, -27.43301270000000258 ) ) ;
#9814 = CARTESIAN_POINT ( 'NONE',  ( -1.249999999999998224, -2.118749998770965703, 2.165063509461097713 ) ) ;
#9815 = AXIS2_PLACEMENT_3D ( 'NONE', #4762, #52, #7266 ) ;
#9816 = CARTESIAN_POINT ( 'NONE',  ( 8.685676809262872666, 100.0000000000000000, 23.43455588346217766 ) ) ;
#9817 = CARTESIAN_POINT ( 'NONE',  ( 3.739209042966564311, 99.99999999999998579, -21.42288334414699591 ) ) ;
#9818 = CARTESIAN_POINT ( 'NONE',  ( 3.105863891863242632, 99.50000000000001421, -22.59672720503480292 ) ) ;
#9819 = CARTESIAN_POINT ( 'NONE',  ( -27.00000000000000355, 4.949999997815051067, -11.18376618407357093 ) ) ;
#9820 = DIRECTION ( 'NONE',  ( -0.000000000000000000, 1.000000000000000000, -0.000000000000000000 ) ) ;
#9821 = CARTESIAN_POINT ( 'NONE',  ( -21.73488407773357167, 100.0000000000000000, -9.647150398373231184 ) ) ;
#9822 = DIRECTION ( 'NONE',  ( -1.067350013832299517E-17, 0.9961946980917455452, 0.08715574274765836016 ) ) ;
#9823 = LINE ( 'NONE', #1862, #8952 ) ;
#9824 = AXIS2_PLACEMENT_3D ( 'NONE', #809, #9097, #5007 ) ;
#9825 = CARTESIAN_POINT ( 'NONE',  ( 4.803433990161294354, 99.50000000000001421, -23.96838578116891583 ) ) ;
#9826 = CARTESIAN_POINT ( 'NONE',  ( -2.256430356249999658, -5.114265559567680697, -0.8212734853698876458 ) ) ;
#9827 = EDGE_LOOP ( 'NONE', ( #2907, #1666, #2376, #3595 ) ) ;
#9828 = ADVANCED_FACE ( 'NONE', ( #5179, #9381 ), #3675, .F. ) ;
#9829 = ORIENTED_EDGE ( 'NONE', *, *, #6012, .T. ) ;
#9830 = CARTESIAN_POINT ( 'NONE',  ( 2.500000000000000444, -0.2624999999999999556, 1.443375672974063439 ) ) ;
#9831 = CARTESIAN_POINT ( 'NONE',  ( -14.76042637754942177, 99.50000000000000000, 16.05242888258284140 ) ) ;
#9832 = CARTESIAN_POINT ( 'NONE',  ( 3.016803124593948393, 99.50000000000001421, -23.20507807535735978 ) ) ;
#9833 = CARTESIAN_POINT ( 'NONE',  ( 19.39806930854667399, 2.549999998907525267, 19.39806930854668465 ) ) ;
#9834 = CARTESIAN_POINT ( 'NONE',  ( 2.500000000000000000, -0.5812499987709658367, -1.443375672974065438 ) ) ;
#9835 = CARTESIAN_POINT ( 'NONE',  ( -20.71654887124055122, 100.0000000000000142, -9.874326132881018125 ) ) ;
#9836 = DIRECTION ( 'NONE',  ( -0.000000000000000000, -1.000000000000000000, -0.000000000000000000 ) ) ;
#9837 = LINE ( 'NONE', #2884, #8580 ) ;
#9838 = VERTEX_POINT ( 'NONE', #7587 ) ;
#9839 = CARTESIAN_POINT ( 'NONE',  ( -21.79396932678589849, 99.50000000000000000, -9.306975108219608828 ) ) ;
#9840 = CARTESIAN_POINT ( 'NONE',  ( -27.43301270000000258, 4.649999998907525800, -3.359575119402369376E-15 ) ) ;
#9841 = CARTESIAN_POINT ( 'NONE',  ( -15.84348323231452049, 99.50000000000000000, 15.18005498687102772 ) ) ;
#9842 = CARTESIAN_POINT ( 'NONE',  ( 0.000000000000000000, 0.000000000000000000, 0.000000000000000000 ) ) ;
#9843 = CARTESIAN_POINT ( 'NONE',  ( 4.320351800798612807, 99.99999999999995737, -21.62386382141117736 ) ) ;
#9844 = CARTESIAN_POINT ( 'NONE',  ( -22.13144646319157260, 99.50000000000001421, -9.428651666388001118 ) ) ;
#9845 = CARTESIAN_POINT ( 'NONE',  ( 3.659868213429061878, 99.50000000000000000, -22.50687739797974274 ) ) ;
#9846 = CARTESIAN_POINT ( 'NONE',  ( -21.18972881998075763, 99.99999999999998579, -9.781869222470191971 ) ) ;
#9847 = ORIENTED_EDGE ( 'NONE', *, *, #2320, .T. ) ;
#9848 = CARTESIAN_POINT ( 'NONE',  ( -2.500000000000000000, -3.581249998770965615, -1.443375672974064106 ) ) ;
#9849 = ORIENTED_EDGE ( 'NONE', *, *, #2683, .T. ) ;
#9850 = ORIENTED_EDGE ( 'NONE', *, *, #9147, .T. ) ;
#9851 = EDGE_CURVE ( 'NONE', #1699, #10071, #3556, .T. ) ;
#9852 = CARTESIAN_POINT ( 'NONE',  ( 0.000000000000000000, 0.000000000000000000, 0.000000000000000000 ) ) ;
#9853 = CARTESIAN_POINT ( 'NONE',  ( 3.204253864046738176, 99.50000000000000000, -22.06071064728738662 ) ) ;
#9854 = CARTESIAN_POINT ( 'NONE',  ( 3.504547665631520648, 99.49999999999997158, -23.10026541809159184 ) ) ;
#9855 =( BOUNDED_CURVE ( )  B_SPLINE_CURVE ( 2, ( #1912, #7318, #5105, #8304, #3343, #4958, #6535, #9722, #987 ),
 .UNSPECIFIED., .F., .F. ) 
 B_SPLINE_CURVE_WITH_KNOTS ( ( 3, 2, 2, 2, 3 ),
 ( 0.7708333333333333703, 0.7777777777777777901, 0.7916666666666666297, 0.8055555555555555802, 0.8125000000000000000 ),
 .UNSPECIFIED. ) 
 CURVE ( )  GEOMETRIC_REPRESENTATION_ITEM ( )  RATIONAL_B_SPLINE_CURVE ( ( 0.9330127018922192983, 0.9330127018922198534, 1.000000000000000000, 0.8660254037844387076, 1.000000000000000000, 0.8660254037844387076, 1.000000000000000000, 0.9330127018922194093, 0.9330127018922194093 ) ) 
 REPRESENTATION_ITEM ( '' )  );
#9856 = CARTESIAN_POINT ( 'NONE',  ( 4.331079892889020400, 99.50000000000000000, -24.67336562508343079 ) ) ;
#9857 = CARTESIAN_POINT ( 'NONE',  ( 8.399337394135656609, 99.49999999999998579, 20.06291166101774692 ) ) ;
#9858 = AXIS2_PLACEMENT_3D ( 'NONE', #2981, #3653, #5330 ) ;
#9859 = CARTESIAN_POINT ( 'NONE',  ( 5.725936192474917696, 99.50000000000000000, 21.08018326417248645 ) ) ;
#9860 = CARTESIAN_POINT ( 'NONE',  ( 4.486604876299897349, 99.50000000000000000, -21.85617661337775885 ) ) ;
#9861 = CARTESIAN_POINT ( 'NONE',  ( 9.431378708427812896, 99.99999999999998579, 21.34379071326255684 ) ) ;
#9862 = ORIENTED_EDGE ( 'NONE', *, *, #887, .F. ) ;
#9863 = LINE ( 'NONE', #342, #4903 ) ;
#9864 = CARTESIAN_POINT ( 'NONE',  ( 11.36312591709336850, 3.399999998907525356, 27.43301269999999903 ) ) ;
#9865 = FACE_OUTER_BOUND ( 'NONE', #3457, .T. ) ;
#9866 = CARTESIAN_POINT ( 'NONE',  ( 3.973150561375555334, 99.99999999999997158, -22.87236500961342855 ) ) ;
#9867 = CARTESIAN_POINT ( 'NONE',  ( 7.729958523985794194, 99.99999999999995737, 20.63140804260154937 ) ) ;
#9868 = ORIENTED_EDGE ( 'NONE', *, *, #592, .F. ) ;
#9869 = CARTESIAN_POINT ( 'NONE',  ( 9.861577898019769250, 99.49999999999995737, 21.03794551367759169 ) ) ;
#9870 = CARTESIAN_POINT ( 'NONE',  ( -27.00000000000001421, 4.249999997815050001, 11.18376618407356382 ) ) ;
#9871 = CARTESIAN_POINT ( 'NONE',  ( 0.000000000000000000, 70.00000000000000000, 23.99999999999999645 ) ) ;
#9872 = DIRECTION ( 'NONE',  ( -1.000000000000000000, 0.000000000000000000, 0.000000000000000000 ) ) ;
#9873 = DIRECTION ( 'NONE',  ( 0.000000000000000000, -1.000000000000000000, 0.000000000000000000 ) ) ;
#9874 = CARTESIAN_POINT ( 'NONE',  ( 2.901827748664965068, 99.99999999999998579, -21.68759887446373469 ) ) ;
#9875 = DIRECTION ( 'NONE',  ( -0.1966827481675937905, 0.000000000000000000, -0.9804671828129909450 ) ) ;
#9876 = CARTESIAN_POINT ( 'NONE',  ( -1.767625397874844694E-16, -2.812500000000000000, -2.886751345948128655 ) ) ;
#9877 = FACE_BOUND ( 'NONE', #2942, .T. ) ;
#9878 = CARTESIAN_POINT ( 'NONE',  ( 2.562556682370379146, -20.00000000000000000, -1.732050807568876749 ) ) ;
#9879 = CARTESIAN_POINT ( 'NONE',  ( 11.36312591709336850, 3.299999998907525711, 27.43301269999999903 ) ) ;
#9880 = CARTESIAN_POINT ( 'NONE',  ( -11.36312591709335962, 0.5999999989075250895, -27.43301270000000258 ) ) ;
#9881 = AXIS2_PLACEMENT_3D ( 'NONE', #3460, #8275, #9062 ) ;
#9882 = AXIS2_PLACEMENT_3D ( 'NONE', #6103, #6831, #8463 ) ;
#9883 = ADVANCED_FACE ( 'NONE', ( #1984 ), #3730, .T. ) ;
#9884 = CARTESIAN_POINT ( 'NONE',  ( -20.63666786535793207, 99.99999999999998579, -10.16306733409737717 ) ) ;
#9885 = PLANE ( 'NONE',  #5662 ) ;
#9886 = DIRECTION ( 'NONE',  ( 0.000000000000000000, 1.000000000000000000, 0.000000000000000000 ) ) ;
#9887 = ORIENTED_EDGE ( 'NONE', *, *, #10251, .F. ) ;
#9888 = CARTESIAN_POINT ( 'NONE',  ( -21.99154324187120579, 99.99999999999994316, -9.362771248264911250 ) ) ;
#9889 = DIRECTION ( 'NONE',  ( -0.000000000000000000, -1.000000000000000000, -0.000000000000000000 ) ) ;
#9890 = CARTESIAN_POINT ( 'NONE',  ( 3.097283534322414766, 100.0000000000000284, -24.18405864774921454 ) ) ;
#9891 = CARTESIAN_POINT ( 'NONE',  ( -15.49723655759404295, 99.49999999999997158, 15.26389171799780264 ) ) ;
#9892 = VECTOR ( 'NONE', #5301, 1000.000000000000000 ) ;
#9893 =( NAMED_UNIT ( * ) SI_UNIT ( $, .STERADIAN. ) SOLID_ANGLE_UNIT ( ) );
#9894 = CARTESIAN_POINT ( 'NONE',  ( 4.187832255138415505, 100.0000000000000142, -21.50835573230103037 ) ) ;
#9895 = CARTESIAN_POINT ( 'NONE',  ( 9.513000527211589841, 99.50000000000000000, 20.35102222961602436 ) ) ;
#9896 = CARTESIAN_POINT ( 'NONE',  ( 9.358681735871565266, 99.99999999999992895, 21.55373624431538815 ) ) ;
#9897 = CARTESIAN_POINT ( 'NONE',  ( -21.00001322343447541, 100.0000000000000142, -9.990026185521596602 ) ) ;
#9898 = ORIENTED_EDGE ( 'NONE', *, *, #6559, .T. ) ;
#9899 = EDGE_CURVE ( 'NONE', #7937, #6736, #2889, .T. ) ;
#9900 = FACE_OUTER_BOUND ( 'NONE', #5598, .T. ) ;
#9901 = VECTOR ( 'NONE', #10103, 1000.000000000000000 ) ;
#9902 = CARTESIAN_POINT ( 'NONE',  ( -1.128215178125000273, -2.128124999385482496, -1.954126010382871259 ) ) ;
#9903 = EDGE_LOOP ( 'NONE', ( #8681, #3393, #277, #5694, #7976 ) ) ;
#9904 = CARTESIAN_POINT ( 'NONE',  ( -4.959819536546781389E-15, 4.599999999999999645, 27.00000000000000355 ) ) ;
#9905 = CARTESIAN_POINT ( 'NONE',  ( 3.202955020264580899, 99.50000000000000000, -21.91595956354277064 ) ) ;
#9906 = CARTESIAN_POINT ( 'NONE',  ( -19.09188309203678457, 4.899999997815050357, -19.09188309203678813 ) ) ;
#9907 = DIRECTION ( 'NONE',  ( -1.000000000000000000, -1.224646799147352961E-16, 0.000000000000000000 ) ) ;
#9908 = ADVANCED_FACE ( 'NONE', ( #9323 ), #1367, .F. ) ;
#9909 = PRESENTATION_LAYER_ASSIGNMENT (  '', '', ( #903 ) ) ;
#9910 = ADVANCED_FACE ( 'NONE', ( #6969 ), #6265, .T. ) ;
#9911 = EDGE_LOOP ( 'NONE', ( #2166, #4671, #9284, #4401 ) ) ;
#9912 = CARTESIAN_POINT ( 'NONE',  ( -27.00000000000000355, 2.750000000000000888, -11.18376618407357270 ) ) ;
#9913 = DIRECTION ( 'NONE',  ( -0.000000000000000000, 1.000000000000000000, -0.000000000000000000 ) ) ;
#9914 = CARTESIAN_POINT ( 'NONE',  ( -22.20893716642541804, 100.0000000000000284, -10.81429252070940272 ) ) ;
#9915 = CARTESIAN_POINT ( 'NONE',  ( 3.282077632710153292, 99.50000000000000000, -23.74569985055724786 ) ) ;
#9916 =( BOUNDED_CURVE ( )  B_SPLINE_CURVE ( 2, ( #3275, #9117, #9015, #10006, #430, #1988, #485, #3569, #8437 ),
 .UNSPECIFIED., .F., .T. ) 
 B_SPLINE_CURVE_WITH_KNOTS ( ( 3, 2, 2, 2, 3 ),
 ( 0.3928571428571428492, 0.4107142857142856984, 0.4285714285714285476, 0.4464285714285714524, 0.4642857142857143016 ),
 .UNSPECIFIED. ) 
 CURVE ( )  GEOMETRIC_REPRESENTATION_ITEM ( )  RATIONAL_B_SPLINE_CURVE ( ( 1.000000000000000000, 0.9238795325112867385, 1.000000000000000000, 0.9238795325112867385, 1.000000000000000000, 0.9238795325112867385, 1.000000000000000000, 0.9238795325112867385, 1.000000000000000000 ) ) 
 REPRESENTATION_ITEM ( '' )  );
#9917 = ORIENTED_EDGE ( 'NONE', *, *, #1615, .F. ) ;
#9918 = CARTESIAN_POINT ( 'NONE',  ( -20.72805389903318130, 99.50000000000000000, -9.848585782927868237 ) ) ;
#9919 = CARTESIAN_POINT ( 'NONE',  ( -11.36312591709337383, 4.899999998907526688, 27.43301269999999548 ) ) ;
#9920 = DIRECTION ( 'NONE',  ( 0.000000000000000000, 0.000000000000000000, 1.000000000000000000 ) ) ;
#9921 = CARTESIAN_POINT ( 'NONE',  ( 2.940631318607589417, 99.50000000000000000, -23.77584808773673331 ) ) ;
#9922 = CARTESIAN_POINT ( 'NONE',  ( 8.133363296361027395, 99.99999999999998579, 19.85287606700953233 ) ) ;
#9923 = ORIENTED_EDGE ( 'NONE', *, *, #2961, .F. ) ;
#9924 = FACE_BOUND ( 'NONE', #3570, .T. ) ;
#9925 = CARTESIAN_POINT ( 'NONE',  ( -27.00000000000000355, 4.999999997815050889, -3.306546357697854128E-15 ) ) ;
#9926 = CARTESIAN_POINT ( 'NONE',  ( -2.500000000000000000, -4.031249998770966236, -1.443375672974064106 ) ) ;
#9927 = MANIFOLD_SOLID_BREP ( 'AdvancedHole1', #2790 ) ;
#9928 = DIRECTION ( 'NONE',  ( -0.000000000000000000, -1.000000000000000000, -0.000000000000000000 ) ) ;
#9929 = CARTESIAN_POINT ( 'NONE',  ( 0.000000000000000000, 104.5000000000000142, 0.000000000000000000 ) ) ;
#9930 = ORIENTED_EDGE ( 'NONE', *, *, #5652, .F. ) ;
#9931 = B_SPLINE_CURVE_WITH_KNOTS ( 'NONE', 3,
 ( #2729, #5866, #1985, #9789, #6649, #1879, #5073, #6552, #3566, #1004, #2782, #2626, #9112, #3405, #1932 ),
 .UNSPECIFIED., .F., .F.,
 ( 4, 1, 1, 1, 1, 1, 1, 1, 1, 1, 1, 1, 4 ),
 ( 0.000000000000000000, 0.1101401978779246588, 0.2116695470404897084, 0.3047824012491699430, 0.3893374185178356539, 0.4648567744508144695, 0.5325800579573772842, 0.5913915682020929321, 0.6424829260185016544, 0.7344861914544180692, 0.8232371011010507500, 0.9113455750355911045, 1.000000000000000000 ),
 .UNSPECIFIED. ) ;
#9932 = CARTESIAN_POINT ( 'NONE',  ( 0.000000000000000000, -15.00000000000000000, 0.000000000000000000 ) ) ;
#9933 = CARTESIAN_POINT ( 'NONE',  ( -1.249999999999998224, -2.174999999999999822, 2.165063509461097713 ) ) ;
#9934 = ORIENTED_EDGE ( 'NONE', *, *, #6148, .F. ) ;
#9935 = CARTESIAN_POINT ( 'NONE',  ( 1.250000000000001110, -2.100000000000000089, 2.165063509461096380 ) ) ;
#9936 = SHAPE_DEFINITION_REPRESENTATION ( #3188, #3375 ) ;
#9937 = FACE_OUTER_BOUND ( 'NONE', #563, .T. ) ;
#9938 = CARTESIAN_POINT ( 'NONE',  ( 2.927917759182871560, 99.49999999999997158, -23.69257214368879261 ) ) ;
#9939 = CARTESIAN_POINT ( 'NONE',  ( 27.43301270000000258, 1.899999998907525134, -11.36312591709336139 ) ) ;
#9940 = CARTESIAN_POINT ( 'NONE',  ( 9.877377282685029372E-16, -0.7874999999999998668, 2.500000000000000000 ) ) ;
#9941 = ORIENTED_EDGE ( 'NONE', *, *, #1140, .F. ) ;
#9942 = CYLINDRICAL_SURFACE ( 'NONE', #4610, 25.15000000000000213 ) ;
#9943 = DIRECTION ( 'NONE',  ( 0.000000000000000000, 1.000000000000000000, 0.000000000000000000 ) ) ;
#9944 = CARTESIAN_POINT ( 'NONE',  ( -27.00000000000000355, 4.149999997815050357, -11.18376618407357270 ) ) ;
#9945 = CIRCLE ( 'NONE', #5612, 0.4999999999999953371 ) ;
#9946 = CARTESIAN_POINT ( 'NONE',  ( 7.746148141271532950, 99.50000000000002842, 20.51930889200067298 ) ) ;
#9947 = FACE_OUTER_BOUND ( 'NONE', #6809, .T. ) ;
#9948 = EDGE_CURVE ( 'NONE', #8813, #3761, #8641, .T. ) ;
#9949 = CARTESIAN_POINT ( 'NONE',  ( -1.250000000000000222, -1.368749998770965925, -2.165063509461096825 ) ) ;
#9950 = CARTESIAN_POINT ( 'NONE',  ( -19.39806930854667755, 0.5499999989075252671, -19.39806930854668110 ) ) ;
#9951 = ADVANCED_FACE ( 'NONE', ( #886 ), #1805, .T. ) ;
#9952 = DIRECTION ( 'NONE',  ( -0.000000000000000000, -0.000000000000000000, -1.000000000000000000 ) ) ;
#9953 = CARTESIAN_POINT ( 'NONE',  ( 9.358681735871565266, 99.49999999999998579, 21.55373624431538815 ) ) ;
#9954 = DIRECTION ( 'NONE',  ( 0.000000000000000000, -0.000000000000000000, -1.000000000000000000 ) ) ;
#9955 = VECTOR ( 'NONE', #6317, 1000.000000000000000 ) ;
#9956 = CARTESIAN_POINT ( 'NONE',  ( -15.98323291606820362, 99.49999999999998579, 16.64087298452848884 ) ) ;
#9957 = CARTESIAN_POINT ( 'NONE',  ( 1.128215178125001161, -1.903124999385482852, 1.954126010382870815 ) ) ;
#9958 = ORIENTED_EDGE ( 'NONE', *, *, #1522, .F. ) ;
#9959 = CARTESIAN_POINT ( 'NONE',  ( -21.96365545856212265, 99.99999999999998579, -9.726658277667754149 ) ) ;
#9960 = CARTESIAN_POINT ( 'NONE',  ( -16.63177974700816009, 99.50000000000000000, 16.59747536361813403 ) ) ;
#9961 = ADVANCED_FACE ( 'NONE', ( #8935 ), #4997, .T. ) ;
#9962 = CARTESIAN_POINT ( 'NONE',  ( 3.973150561375555334, 99.50000000000000000, -22.87236500961342855 ) ) ;
#9963 = CARTESIAN_POINT ( 'NONE',  ( 0.000000000000000000, 71.18660744634364335, 0.000000000000000000 ) ) ;
#9964 = VERTEX_POINT ( 'NONE', #2510 ) ;
#9965 = CARTESIAN_POINT ( 'NONE',  ( -16.37951318544778445, 99.49999999999997158, 15.41600550949200077 ) ) ;
#9966 = CIRCLE ( 'NONE', #9477, 7.500000000000000000 ) ;
#9967 = CARTESIAN_POINT ( 'NONE',  ( 3.207057600658871355, 99.50000000000000000, -22.07913334414698880 ) ) ;
#9968 = EDGE_CURVE ( 'NONE', #969, #10097, #255, .T. ) ;
#9969 = CARTESIAN_POINT ( 'NONE',  ( -16.91946509138130139, 100.0000000000000142, 15.98858002463268413 ) ) ;
#9970 = CARTESIAN_POINT ( 'NONE',  ( 3.478562133589548910, 99.49999999999997158, -24.13114810667639532 ) ) ;
#9971 = ORIENTED_EDGE ( 'NONE', *, *, #2318, .F. ) ;
#9972 = FACE_OUTER_BOUND ( 'NONE', #4652, .T. ) ;
#9973 = CARTESIAN_POINT ( 'NONE',  ( -19.39806930854667755, 3.849999998907525089, -19.39806930854668110 ) ) ;
#9974 = DIRECTION ( 'NONE',  ( -0.000000000000000000, 1.000000000000000000, -0.000000000000000000 ) ) ;
#9975 = CARTESIAN_POINT ( 'NONE',  ( 9.910564025336874749, 100.0000000000000000, 20.75459158945058036 ) ) ;
#9976 = CARTESIAN_POINT ( 'NONE',  ( -9.703070624755296135E-15, -3.487499999999999822, 2.500000000000000444 ) ) ;
#9977 = ORIENTED_EDGE ( 'NONE', *, *, #9123, .T. ) ;
#9978 = CARTESIAN_POINT ( 'NONE',  ( 9.834295043520187463, 99.50000000000002842, 21.14079655679390513 ) ) ;
#9979 = CARTESIAN_POINT ( 'NONE',  ( 11.18376618407357626, 4.449999997815051067, 27.00000000000000000 ) ) ;
#9980 = CARTESIAN_POINT ( 'NONE',  ( 27.00000000000000355, 3.250000000000000444, -11.18376618407356915 ) ) ;
#9981 =( BOUNDED_CURVE ( )  B_SPLINE_CURVE ( 2, ( #5966, #9158, #1978, #3354, #4970, #8170, #1824, #5019, #8216 ),
 .UNSPECIFIED., .F., .T. ) 
 B_SPLINE_CURVE_WITH_KNOTS ( ( 3, 2, 2, 2, 3 ),
 ( 0.2291666666666666574, 0.2361111111111111049, 0.2500000000000000000, 0.2638888888888888951, 0.2708333333333333703 ),
 .UNSPECIFIED. ) 
 CURVE ( )  GEOMETRIC_REPRESENTATION_ITEM ( )  RATIONAL_B_SPLINE_CURVE ( ( 0.9330127018922194093, 0.9330127018922194093, 1.000000000000000000, 0.8660254037844387076, 1.000000000000000000, 0.8660254037844387076, 1.000000000000000000, 0.9330127018922190762, 0.9330127018922194093 ) ) 
 REPRESENTATION_ITEM ( '' )  );
#9982 = CARTESIAN_POINT ( 'NONE',  ( 0.000000000000000000, 0.000000000000000000, 0.000000000000000000 ) ) ;
#9983 = FILL_AREA_STYLE ('',( #7567 ) ) ;
#9984 = EDGE_LOOP ( 'NONE', ( #92, #3086, #8762, #382 ) ) ;
#9985 = CARTESIAN_POINT ( 'NONE',  ( 4.829054701479813083, 100.0000000000000000, -23.91032069601275367 ) ) ;
#9986 = CARTESIAN_POINT ( 'NONE',  ( -19.39806930854667755, 1.449999998907525178, -19.39806930854668110 ) ) ;
#9987 = ORIENTED_EDGE ( 'NONE', *, *, #8566, .F. ) ;
#9988 = ADVANCED_FACE ( 'NONE', ( #5701 ), #8516, .T. ) ;
#9989 = CARTESIAN_POINT ( 'NONE',  ( 1.249999999999999334, -1.949999999999999956, -2.165063509461096825 ) ) ;
#9990 = CARTESIAN_POINT ( 'NONE',  ( -1.915121305771201099, 0.000000000000000000, -1.606956870666170323 ) ) ;
#9991 = CARTESIAN_POINT ( 'NONE',  ( 4.786228327491941173E-16, -1.940624999385482718, 2.605501347177161087 ) ) ;
#9992 = CARTESIAN_POINT ( 'NONE',  ( -11.36312591709337383, 2.399999998907525356, 27.43301269999999548 ) ) ;
#9993 = LINE ( 'NONE', #415, #4541 ) ;
#9994 = ORIENTED_EDGE ( 'NONE', *, *, #2350, .F. ) ;
#9995 = CARTESIAN_POINT ( 'NONE',  ( -16.60513711880302878, 100.0000000000000000, 15.15667007515659570 ) ) ;
#9996 = VECTOR ( 'NONE', #6746, 1000.000000000000000 ) ;
#9997 = CARTESIAN_POINT ( 'NONE',  ( 7.500000000000000000, 105.0000000000000142, -0.9999999999999997780 ) ) ;
#9998 = CARTESIAN_POINT ( 'NONE',  ( 7.753999887479250397, 100.0000000000000000, 20.97676509141502166 ) ) ;
#9999 = CARTESIAN_POINT ( 'NONE',  ( 3.597125852879613728, 99.99999999999998579, -24.22990373345680126 ) ) ;
#10000 = DIRECTION ( 'NONE',  ( 0.2499845035238856816, 0.000000000000000000, -0.9682498375925071565 ) ) ;
#10001 = EDGE_LOOP ( 'NONE', ( #8705, #1215, #9421, #4317 ) ) ;
#10002 = CARTESIAN_POINT ( 'NONE',  ( -2.256430356250000102, -0.6281249993854828295, -1.302750673588580321 ) ) ;
#10003 = CARTESIAN_POINT ( 'NONE',  ( -11.36312591709337383, 2.399999998907525356, 27.43301269999999548 ) ) ;
#10004 = CARTESIAN_POINT ( 'NONE',  ( -16.56926954694585774, 99.50000000000001421, 15.12296757606276643 ) ) ;
#10005 = CARTESIAN_POINT ( 'NONE',  ( 3.212364564527730337, 99.50000000000000000, -22.10366694310577884 ) ) ;
#10006 = CARTESIAN_POINT ( 'NONE',  ( 26.99999999999999645, 2.350000000000000533, 11.18376618407358691 ) ) ;
#10007 = ORIENTED_EDGE ( 'NONE', *, *, #3329, .T. ) ;
#10008 = DIRECTION ( 'NONE',  ( -0.000000000000000000, -1.000000000000000000, -0.000000000000000000 ) ) ;
#10009 = CARTESIAN_POINT ( 'NONE',  ( -1.595409442497313560E-16, -2.615624999385482319, -2.605501347177161087 ) ) ;
#10010 = ORIENTED_EDGE ( 'NONE', *, *, #8691, .F. ) ;
#10011 = CARTESIAN_POINT ( 'NONE',  ( 0.000000000000000000, 85.00000000000000000, -20.00000000000000000 ) ) ;
#10012 = DIRECTION ( 'NONE',  ( -0.000000000000000000, 1.000000000000000000, -0.000000000000000000 ) ) ;
#10013 = DIRECTION ( 'NONE',  ( -0.000000000000000000, -1.000000000000000000, -0.000000000000000000 ) ) ;
#10014 = CARTESIAN_POINT ( 'NONE',  ( 2.924645347134957163, 100.0000000000000142, -23.60918035669702064 ) ) ;
#10015 = ORIENTED_EDGE ( 'NONE', *, *, #8659, .F. ) ;
#10016 = EDGE_CURVE ( 'NONE', #1992, #5243, #5838, .T. ) ;
#10017 = CARTESIAN_POINT ( 'NONE',  ( 4.200543313440712190, 99.50000000000000000, -21.13206004899810608 ) ) ;
#10018 = CARTESIAN_POINT ( 'NONE',  ( -2.499999999999999112, -2.606249998770965526, 1.443375672974065882 ) ) ;
#10019 = DIRECTION ( 'NONE',  ( 0.05468478504300072762, 0.000000000000000000, 0.9985036676371302766 ) ) ;
#10020 = ORIENTED_EDGE ( 'NONE', *, *, #4409, .T. ) ;
#10021 = CARTESIAN_POINT ( 'NONE',  ( 0.000000000000000000, 70.00000000000000000, 0.000000000000000000 ) ) ;
#10022 = CARTESIAN_POINT ( 'NONE',  ( 19.39806930854668110, 3.649999998907525356, -19.39806930854668110 ) ) ;
#10023 = CARTESIAN_POINT ( 'NONE',  ( -2.500000000000000000, -4.973640350848739899, -0.9099175284171375777 ) ) ;
#10024 = CARTESIAN_POINT ( 'NONE',  ( 9.902568905804752575, 99.49999999999998579, 20.48863403721516363 ) ) ;
#10025 = ORIENTED_EDGE ( 'NONE', *, *, #1194, .F. ) ;
#10026 = CARTESIAN_POINT ( 'NONE',  ( 1.670949432750432147E-15, 5.433333331876700534, -27.28867513333333505 ) ) ;
#10027 = VECTOR ( 'NONE', #6888, 1000.000000000000000 ) ;
#10028 = CARTESIAN_POINT ( 'NONE',  ( 4.988497440555089923, 99.50000000000000000, -24.29977663856455194 ) ) ;
#10029 = FILL_AREA_STYLE ('',( #1346 ) ) ;
#10030 = CYLINDRICAL_SURFACE ( 'NONE', #8003, 7.500000000000000000 ) ;
#10031 = EDGE_LOOP ( 'NONE', ( #6760, #4167, #8565, #2549 ) ) ;
#10032 = CARTESIAN_POINT ( 'NONE',  ( 0.000000000000000000, 73.81339255365637086, 23.99999999999999645 ) ) ;
#10033 = CARTESIAN_POINT ( 'NONE',  ( 1.679787559701184688E-15, 2.149999998907525356, -27.43301270000000258 ) ) ;
#10034 = ORIENTED_EDGE ( 'NONE', *, *, #9528, .F. ) ;
#10035 = B_SPLINE_CURVE_WITH_KNOTS ( 'NONE', 3,
 ( #4309, #7494, #5929, #4260, #1224, #4415, #1945, #7600, #9854, #1169, #333, #1841, #9176, #3689, #5832, #9962, #4467, #8236, #9024 ),
 .UNSPECIFIED., .F., .F.,
 ( 4, 1, 1, 1, 1, 1, 1, 1, 1, 1, 1, 1, 1, 1, 1, 1, 4 ),
 ( 0.000000000000000000, 0.07039602572822099835, 0.1400447079551435658, 0.2099027554305550880, 0.2826152692239142783, 0.3556467613428230812, 0.4271065942619623468, 0.4986634349892335449, 0.5720141774457471184, 0.6112909118483191850, 0.6543288624652392471, 0.7009162800881839628, 0.7518538071550001645, 0.8072437197097745987, 0.8671654997918389896, 0.9315515937071113806, 1.000000000000000000 ),
 .UNSPECIFIED. ) ;
#10036 = CARTESIAN_POINT ( 'NONE',  ( 1.249999999999999334, -1.050000000000000044, -2.165063509461096825 ) ) ;
#10037 = CARTESIAN_POINT ( 'NONE',  ( 0.000000000000000000, 72.50000000000001421, 0.000000000000000000 ) ) ;
#10038 = CARTESIAN_POINT ( 'NONE',  ( 3.551917533706515417, 99.99999999999998579, -21.11785906961830150 ) ) ;
#10039 = CARTESIAN_POINT ( 'NONE',  ( 2.256430356249999658, -0.8906249993854827851, -1.302750673588581432 ) ) ;
#10040 = ADVANCED_FACE ( 'NONE', ( #9032 ), #1849, .F. ) ;
#10041 = CARTESIAN_POINT ( 'NONE',  ( 27.43301270000000258, 5.049999998907525267, 0.000000000000000000 ) ) ;
#10042 = CARTESIAN_POINT ( 'NONE',  ( 11.36312591709336850, 0.9999999989075254447, 27.43301269999999903 ) ) ;
#10043 = ADVANCED_FACE ( 'NONE', ( #9084 ), #1902, .T. ) ;
#10044 = CARTESIAN_POINT ( 'NONE',  ( -16.18394139941567644, 100.0000000000000000, 16.57042731130403723 ) ) ;
#10045 = CARTESIAN_POINT ( 'NONE',  ( -0.6698729810778081273, -3.001346188203299903, 2.499999999999999112 ) ) ;
#10046 = CARTESIAN_POINT ( 'NONE',  ( 1.653273178848927064E-15, 3.999999997815050889, -27.00000000000000355 ) ) ;
#10047 = CARTESIAN_POINT ( 'NONE',  ( -16.34436021381890924, 100.0000000000000000, 15.38072013554846151 ) ) ;
#10048 = VERTEX_POINT ( 'NONE', #2856 ) ;
#10049 = CARTESIAN_POINT ( 'NONE',  ( 2.256430356250000102, -2.165624999385483029, -2.763330213280484622E-16 ) ) ;
#10050 = DIRECTION ( 'NONE',  ( -0.000000000000000000, 1.000000000000000000, -0.000000000000000000 ) ) ;
#10051 = ORIENTED_EDGE ( 'NONE', *, *, #6709, .T. ) ;
#10052 = CARTESIAN_POINT ( 'NONE',  ( 0.000000000000000000, 97.50000000000000000, 0.000000000000000000 ) ) ;
#10053 = CARTESIAN_POINT ( 'NONE',  ( -19.39806930854668465, 1.549999998907525267, 19.39806930854667755 ) ) ;
#10054 = SURFACE_SIDE_STYLE ('',( #539 ) ) ;
#10055 = CARTESIAN_POINT ( 'NONE',  ( 0.000000000000000000, 71.18660744634364335, 0.000000000000000000 ) ) ;
#10056 = VECTOR ( 'NONE', #7546, 1000.000000000000114 ) ;
#10057 = CIRCLE ( 'NONE', #5203, 23.99999999999999645 ) ;
#10058 = CARTESIAN_POINT ( 'NONE',  ( 9.526713201929464248, 99.50000000000000000, 20.38668308130821671 ) ) ;
#10059 = FACE_OUTER_BOUND ( 'NONE', #10328, .T. ) ;
#10060 = ORIENTED_EDGE ( 'NONE', *, *, #6418, .F. ) ;
#10061 = ORIENTED_EDGE ( 'NONE', *, *, #1765, .F. ) ;
#10062 = CARTESIAN_POINT ( 'NONE',  ( -1.728530063377412107, -5.141148402510967053, -1.450400555903694988 ) ) ;
#10063 = CARTESIAN_POINT ( 'NONE',  ( -2.256430356249999214, -1.565624999385482718, 1.302750673588581876 ) ) ;
#10064 = EDGE_LOOP ( 'NONE', ( #2078, #2842, #7645, #3842, #5796, #2046, #8415, #8103 ) ) ;
#10065 = CARTESIAN_POINT ( 'NONE',  ( -21.94169572595625795, 99.99999999999997158, -9.715372641902229489 ) ) ;
#10066 = CARTESIAN_POINT ( 'NONE',  ( 0.6698729810778069060, -0.5825961894323341550, -2.500000000000000000 ) ) ;
#10067 = CARTESIAN_POINT ( 'NONE',  ( -7.500000000000000000, 104.5000000000000142, -3.000000000000000000 ) ) ;
#10068 = CARTESIAN_POINT ( 'NONE',  ( -1.128215178125000273, -0.3281249993854828961, -1.954126010382871259 ) ) ;
#10069 = CARTESIAN_POINT ( 'NONE',  ( -2.562556682370380035, -20.00000000000000000, 1.732050807568878303 ) ) ;
#10070 = VECTOR ( 'NONE', #8503, 1000.000000000000000 ) ;
#10071 = VERTEX_POINT ( 'NONE', #395 ) ;
#10072 = CARTESIAN_POINT ( 'NONE',  ( 0.000000000000000000, 0.000000000000000000, 0.000000000000000000 ) ) ;
#10073 = CARTESIAN_POINT ( 'NONE',  ( -1.250000000000000222, -2.718749998770965792, -2.165063509461096825 ) ) ;
#10074 = DIRECTION ( 'NONE',  ( 0.000000000000000000, 0.000000000000000000, -1.000000000000000000 ) ) ;
#10075 = ORIENTED_EDGE ( 'NONE', *, *, #9606, .T. ) ;
#10076 = FACE_OUTER_BOUND ( 'NONE', #6911, .T. ) ;
#10077 = VECTOR ( 'NONE', #8247, 1000.000000000000000 ) ;
#10078 = CARTESIAN_POINT ( 'NONE',  ( 1.679787559701184688E-15, 2.949999998907525178, -27.43301270000000258 ) ) ;
#10079 = CARTESIAN_POINT ( 'NONE',  ( 4.786228327491941173E-16, -0.9281249993854828739, 2.605501347177161087 ) ) ;
#10080 = EDGE_CURVE ( 'NONE', #7765, #6494, #6880, .T. ) ;
#10081 = LINE ( 'NONE', #6827, #4259 ) ;
#10082 = ORIENTED_EDGE ( 'NONE', *, *, #4045, .T. ) ;
#10083 = CARTESIAN_POINT ( 'NONE',  ( -21.30033281797529909, 100.0000000000000284, -9.345151174687854834 ) ) ;
#10084 = PLANE ( 'NONE',  #7373 ) ;
#10085 = LINE ( 'NONE', #2921, #6367 ) ;
#10086 = CARTESIAN_POINT ( 'NONE',  ( 0.000000000000000000, 0.000000000000000000, 0.000000000000000000 ) ) ;
#10087 = ORIENTED_EDGE ( 'NONE', *, *, #5646, .F. ) ;
#10088 = CARTESIAN_POINT ( 'NONE',  ( -15.69732130854469432, 99.50000000000001421, 15.19348709373450035 ) ) ;
#10089 = CARTESIAN_POINT ( 'NONE',  ( -27.43301270000000258, 2.299999998907525267, -11.36312591709336317 ) ) ;
#10090 = VERTEX_POINT ( 'NONE', #5201 ) ;
#10091 = CARTESIAN_POINT ( 'NONE',  ( -2.500000000000000000, -1.387499999999999956, -1.443375672974064106 ) ) ;
#10092 = CARTESIAN_POINT ( 'NONE',  ( -16.56928979259283352, 100.0000000000000284, 16.65656195153832897 ) ) ;
#10093 = DIRECTION ( 'NONE',  ( -0.000000000000000000, 1.000000000000000000, -0.000000000000000000 ) ) ;
#10094 = CARTESIAN_POINT ( 'NONE',  ( -1.128215178124998497, -1.978124999385482807, 1.954126010382872147 ) ) ;
#10095 = CARTESIAN_POINT ( 'NONE',  ( 3.306546357697854128E-15, 100.0000000000000000, 27.00000000000000355 ) ) ;
#10096 = CARTESIAN_POINT ( 'NONE',  ( 27.43301269999999548, 1.899999998907525356, 11.36312591709337738 ) ) ;
#10097 = VERTEX_POINT ( 'NONE', #7610 ) ;
#10098 = UNCERTAINTY_MEASURE_WITH_UNIT (LENGTH_MEASURE( 1.000000000000000082E-05 ), #1933, 'distance_accuracy_value', 'NONE');
#10099 = CARTESIAN_POINT ( 'NONE',  ( 2.500000000000000444, -2.062499999999999556, 1.443375672974063439 ) ) ;
#10100 = EDGE_CURVE ( 'NONE', #7488, #3916, #5096, .T. ) ;
#10101 = VECTOR ( 'NONE', #4675, 1000.000000000000000 ) ;
#10102 = CARTESIAN_POINT ( 'NONE',  ( 4.143207896384923039, 99.99999999999998579, -24.36264353342416911 ) ) ;
#10103 = DIRECTION ( 'NONE',  ( -0.8547548816071318667, 0.000000000000000000, 0.5190318799156541374 ) ) ;
#10104 = PRODUCT_DEFINITION_SHAPE ( 'NONE', 'NONE',  #10367 ) ;
#10105 = DIRECTION ( 'NONE',  ( 0.000000000000000000, 0.000000000000000000, -1.000000000000000000 ) ) ;
#10106 = EDGE_LOOP ( 'NONE', ( #8801, #654, #6778, #2036 ) ) ;
#10107 = CARTESIAN_POINT ( 'NONE',  ( -2.256430356250000102, -1.978124999385482807, -1.302750673588580321 ) ) ;
#10108 = FACE_OUTER_BOUND ( 'NONE', #7699, .T. ) ;
#10109 = ORIENTED_EDGE ( 'NONE', *, *, #4349, .F. ) ;
#10110 = ADVANCED_FACE ( 'NONE', ( #5150 ), #3589, .T. ) ;
#10111 = DIRECTION ( 'NONE',  ( -0.04357787137382917314, -0.9961946980917455452, -0.07547908730517351172 ) ) ;
#10112 = CARTESIAN_POINT ( 'NONE',  ( -11.36312591709335962, 3.699999998907525622, -27.43301270000000258 ) ) ;
#10113 = ADVANCED_FACE ( 'NONE', ( #10076 ), #2913, .T. ) ;
#10114 = CARTESIAN_POINT ( 'NONE',  ( 1.249999999999999334, -2.793749998770965526, -2.165063509461096825 ) ) ;
#10115 = CARTESIAN_POINT ( 'NONE',  ( -11.18376618407356560, 1.849999999999999867, -27.00000000000000355 ) ) ;
#10116 = DIRECTION ( 'NONE',  ( -0.000000000000000000, -1.000000000000000000, -0.000000000000000000 ) ) ;
#10117 = ORIENTED_EDGE ( 'NONE', *, *, #9606, .F. ) ;
#10119 = EDGE_CURVE ( 'NONE', #4452, #4542, #6567, .T. ) ;
#10118 = VECTOR ( 'NONE', #5565, 1000.000000000000000 ) ;
#10120 = CARTESIAN_POINT ( 'NONE',  ( 8.064245308217579122, 99.49999999999998579, 20.64099956338070641 ) ) ;
#10121 = CARTESIAN_POINT ( 'NONE',  ( 1.128215178124999607, -0.8531249993854828073, -1.954126010382871259 ) ) ;
#10122 = VERTEX_POINT ( 'NONE', #6774 ) ;
#10123 = CARTESIAN_POINT ( 'NONE',  ( 4.386516977709190357, 99.50000000000004263, -24.31220192127581825 ) ) ;
#10124 = CARTESIAN_POINT ( 'NONE',  ( -19.39806930854667755, 0.5499999989075252671, -19.39806930854668110 ) ) ;
#10125 = CARTESIAN_POINT ( 'NONE',  ( -21.80427673524616239, 99.50000000000000000, -9.663674634844889866 ) ) ;
#10126 = CIRCLE ( 'NONE', #8278, 23.99999999999999645 ) ;
#10127 = EDGE_CURVE ( 'NONE', #3209, #6813, #9419, .T. ) ;
#10128 = CARTESIAN_POINT ( 'NONE',  ( 2.256430356250000546, -1.865624999385482985, 1.302750673588579877 ) ) ;
#10129 = LINE ( 'NONE', #10069, #4372 ) ;
#10130 = DIRECTION ( 'NONE',  ( 0.000000000000000000, -1.000000000000000000, 0.000000000000000000 ) ) ;
#10131 = AXIS2_PLACEMENT_3D ( 'NONE', #9559, #10296, #3129 ) ;
#10132 = ADVANCED_FACE ( 'NONE', ( #9972 ), #447, .F. ) ;
#10133 = DIRECTION ( 'NONE',  ( -0.000000000000000000, 1.000000000000000000, -0.000000000000000000 ) ) ;
#10134 = CARTESIAN_POINT ( 'NONE',  ( -4.357666448243394824E-15, -2.531249998770965348, 2.500000000000000000 ) ) ;
#10135 = DIRECTION ( 'NONE',  ( -0.000000000000000000, -1.000000000000000000, -0.000000000000000000 ) ) ;
#10136 = ORIENTED_EDGE ( 'NONE', *, *, #5142, .T. ) ;
#10137 = CARTESIAN_POINT ( 'NONE',  ( -21.98271324694694329, 100.0000000000000000, -11.39207625356720222 ) ) ;
#10138 = CARTESIAN_POINT ( 'NONE',  ( 1.249999999999999334, -4.200000000000000178, -2.165063509461096825 ) ) ;
#10139 = CARTESIAN_POINT ( 'NONE',  ( -1.128215178125000273, -2.465624999385482852, -1.954126010382871259 ) ) ;
#10140 = CARTESIAN_POINT ( 'NONE',  ( 9.723125805078051798, 99.99999999999998579, 21.50134635983626907 ) ) ;
#10141 = ORIENTED_EDGE ( 'NONE', *, *, #4254, .T. ) ;
#10142 = CYLINDRICAL_SURFACE ( 'NONE', #5253, 0.4999999999999953371 ) ;
#10143 = VECTOR ( 'NONE', #8130, 1000.000000000000000 ) ;
#10144 = CARTESIAN_POINT ( 'NONE',  ( 8.644881627383616873, 99.99999999999995737, 19.60534525227960145 ) ) ;
#10145 =( BOUNDED_CURVE ( )  B_SPLINE_CURVE ( 2, ( #1157, #6912, #9208, #1208, #6073, #1317, #9949, #7758, #4402 ),
 .UNSPECIFIED., .F., .T. ) 
 B_SPLINE_CURVE_WITH_KNOTS ( ( 3, 2, 2, 2, 3 ),
 ( 0.1458333333333333426, 0.1527777777777777901, 0.1666666666666666574, 0.1805555555555555525, 0.1875000000000000000 ),
 .UNSPECIFIED. ) 
 CURVE ( )  GEOMETRIC_REPRESENTATION_ITEM ( )  RATIONAL_B_SPLINE_CURVE ( ( 0.9330127018922194093, 0.9330127018922194093, 1.000000000000000000, 0.8660254037844387076, 1.000000000000000000, 0.8660254037844387076, 1.000000000000000000, 0.9330127018922194093, 0.9330127018922194093 ) ) 
 REPRESENTATION_ITEM ( '' )  );
#10146 =( LENGTH_UNIT ( ) NAMED_UNIT ( * ) SI_UNIT ( .MILLI., .METRE. ) );
#10147 = CARTESIAN_POINT ( 'NONE',  ( -21.30928386698190025, 100.0000000000000000, -11.02857376369709996 ) ) ;
#10148 = VERTEX_POINT ( 'NONE', #9289 ) ;
#10149 = DIRECTION ( 'NONE',  ( -0.000000000000000000, 1.000000000000000000, -0.000000000000000000 ) ) ;
#10150 = CLOSED_SHELL ( 'NONE', ( #5933, #9554, #784, #2375, #8378, #6413, #10113, #553, #7339, #6269 ) ) ;
#10151 = ORIENTED_EDGE ( 'NONE', *, *, #6453, .T. ) ;
#10152 = APPLICATION_CONTEXT ( 'automotive_design' ) ;
#10153 = VECTOR ( 'NONE', #664, 1000.000000000000000 ) ;
#10154 = VECTOR ( 'NONE', #8980, 1000.000000000000000 ) ;
#10155 = CARTESIAN_POINT ( 'NONE',  ( 2.500000000000000000, -2.924999999999999822, -3.061616997868383141E-16 ) ) ;
#10156 = PRODUCT_CONTEXT ( 'NONE', #3521, 'mechanical' ) ;
#10157 = LINE ( 'NONE', #7849, #1433 ) ;
#10158 = CARTESIAN_POINT ( 'NONE',  ( 1.128215178124999607, -1.303124999385482985, -1.954126010382871259 ) ) ;
#10159 = CARTESIAN_POINT ( 'NONE',  ( -16.76168403648438243, 99.50000000000002842, 16.44483764528499847 ) ) ;
#10160 = CARTESIAN_POINT ( 'NONE',  ( 27.43301269999999548, 2.699999998907525178, 11.36312591709337738 ) ) ;
#10161 = CARTESIAN_POINT ( 'NONE',  ( 8.465276868207817884, 100.0000000000000142, 19.66343818277063704 ) ) ;
#10162 = CARTESIAN_POINT ( 'NONE',  ( -1.249999999999998224, -3.524999999999999467, 2.165063509461097713 ) ) ;
#10163 = DIRECTION ( 'NONE',  ( -0.9851965920526258857, 0.000000000000000000, -0.1714283378204774222 ) ) ;
#10164 = CARTESIAN_POINT ( 'NONE',  ( 3.681717055787076642, 99.50000000000000000, -21.09125273517263111 ) ) ;
#10165 = EDGE_CURVE ( 'NONE', #6494, #4294, #9863, .T. ) ;
#10166 = CARTESIAN_POINT ( 'NONE',  ( -15.69732130854469432, 100.0000000000000142, 15.19348709373450035 ) ) ;
#10167 = CARTESIAN_POINT ( 'NONE',  ( 2.256430356250000102, -1.265624999385482896, -2.763330213280484622E-16 ) ) ;
#10168 = DIRECTION ( 'NONE',  ( -0.000000000000000000, -1.000000000000000000, -0.000000000000000000 ) ) ;
#10169 = ORIENTED_EDGE ( 'NONE', *, *, #1891, .F. ) ;
#10170 = CARTESIAN_POINT ( 'NONE',  ( -1.128215178125000273, -0.2156249993854829350, -1.954126010382871259 ) ) ;
#10171 = CARTESIAN_POINT ( 'NONE',  ( 11.36312591709336139, 1.199999998907525178, -27.43301270000000258 ) ) ;
#10172 =( NAMED_UNIT ( * ) SI_UNIT ( $, .STERADIAN. ) SOLID_ANGLE_UNIT ( ) );
#10173 = ORIENTED_EDGE ( 'NONE', *, *, #2174, .T. ) ;
#10174 = LINE ( 'NONE', #2892, #3932 ) ;
#10175 = CARTESIAN_POINT ( 'NONE',  ( 19.09188309203678102, 2.299999999999999822, 19.09188309203678813 ) ) ;
#10176 = CARTESIAN_POINT ( 'NONE',  ( 0.000000000000000000, 100.0000000000000000, 0.000000000000000000 ) ) ;
#10177 = VERTEX_POINT ( 'NONE', #1285 ) ;
#10178 = CARTESIAN_POINT ( 'NONE',  ( -16.54512803120131181, 99.99999999999995737, 16.13427955854364626 ) ) ;
#10179 = CARTESIAN_POINT ( 'NONE',  ( 0.000000000000000000, -15.00000000000000000, 0.000000000000000000 ) ) ;
#10180 = ORIENTED_EDGE ( 'NONE', *, *, #4726, .T. ) ;
#10181 = CARTESIAN_POINT ( 'NONE',  ( -2.256430356249999214, -3.815624999385482941, 1.302750673588581876 ) ) ;
#10182 = ORIENTED_EDGE ( 'NONE', *, *, #9027, .F. ) ;
#10183 = EDGE_LOOP ( 'NONE', ( #2454, #1788, #7754, #1294 ) ) ;
#10184 = VECTOR ( 'NONE', #7843, 999.9999999999998863 ) ;
#10185 = DIRECTION ( 'NONE',  ( -1.000000000000000000, 0.000000000000000000, 0.000000000000000000 ) ) ;
#10186 = CARTESIAN_POINT ( 'NONE',  ( -1.728529299398585906, -5.253648441416169490, -1.450401466387756244 ) ) ;
#10187 = CARTESIAN_POINT ( 'NONE',  ( 4.786228327491940187E-16, -1.940624999385482718, 2.605501347177161087 ) ) ;
#10188 = CARTESIAN_POINT ( 'NONE',  ( 2.927917759182871560, 99.99999999999997158, -23.69257214368879261 ) ) ;
#10189 = CARTESIAN_POINT ( 'NONE',  ( -2.500000000000000000, -0.3937499987709658922, 0.000000000000000000 ) ) ;
#10190 = EDGE_CURVE ( 'NONE', #8208, #7672, #7721, .T. ) ;
#10191 = B_SPLINE_CURVE_WITH_KNOTS ( 'NONE', 3,
 ( #3300, #4763, #9680, #1241, #9042, #5899, #1136, #4329, #6835, #2817, #250, #2012, #1860, #8358, #2657, #1189, #5847, #9095, #6000 ),
 .UNSPECIFIED., .F., .F.,
 ( 4, 1, 1, 1, 1, 1, 1, 1, 1, 1, 1, 1, 1, 1, 1, 1, 4 ),
 ( 0.000000000000000000, 0.07039602572822099835, 0.1400447079551435658, 0.2099027554305550880, 0.2826152692239142783, 0.3556467613428230812, 0.4271065942619623468, 0.4986634349892335449, 0.5720141774457471184, 0.6112909118483191850, 0.6543288624652392471, 0.7009162800881839628, 0.7518538071550001645, 0.8072437197097745987, 0.8671654997918389896, 0.9315515937071113806, 1.000000000000000000 ),
 .UNSPECIFIED. ) ;
#10192 = EDGE_CURVE ( 'NONE', #9616, #717, #7667, .T. ) ;
#10193 = CARTESIAN_POINT ( 'NONE',  ( -2.500000000000000000, -3.093749998770965348, 0.000000000000000000 ) ) ;
#10194 = EDGE_LOOP ( 'NONE', ( #3304, #6890, #5332, #3806 ) ) ;
#10195 = CARTESIAN_POINT ( 'NONE',  ( -2.500000000000000000, -2.643749998770965615, 0.000000000000000000 ) ) ;
#10196 = CARTESIAN_POINT ( 'NONE',  ( 27.00000000000000355, 0.8500000000000001998, -11.18376618407356915 ) ) ;
#10197 = VERTEX_POINT ( 'NONE', #5991 ) ;
#10198 = CARTESIAN_POINT ( 'NONE',  ( -0.6698729810778105698, -4.351346188203299548, 2.499999999999997780 ) ) ;
#10199 = CARTESIAN_POINT ( 'NONE',  ( -1.595409442497313560E-16, -1.153124999385483074, -2.605501347177161087 ) ) ;
#10200 = B_SPLINE_SURFACE_WITH_KNOTS ( 'NONE', 3, 1, ( 
 ( #9071, #1990 ),
 ( #9120, #1886 ),
 ( #5135, #6758 ),
 ( #7651, #5080 ),
 ( #378, #488 ),
 ( #6865, #2736 ),
 ( #6083, #1216 ),
 ( #9956, #2789 ),
 ( #9273, #1111 ),
 ( #4303, #8387 ),
 ( #6355, #3065 ),
 ( #2219, #3015 ),
 ( #9548, #3895 ),
 ( #2326, #9447 ),
 ( #5572, #6192 ),
 ( #2956, #8715 ),
 ( #9390, #7870 ),
 ( #1379, #2374 ),
 ( #7767, #5523 ) ),
 .UNSPECIFIED., .F., .F., .F.,
 ( 4, 1, 1, 1, 1, 1, 1, 1, 1, 1, 1, 1, 1, 1, 1, 1, 4 ),
 ( 2, 2 ),
 ( 0.000000000000000000, 0.06473117683888822416, 0.1283191082976379849, 0.1900130092022370987, 0.2509653124206144836, 0.3118694605430146760, 0.3735603890354366463, 0.4359106579620777855, 0.5007804971236301528, 0.5656503362851855732, 0.6280858374182423098, 0.6899222460797727052, 0.7510277903999277305, 0.8114330998898260372, 0.8726106248506092511, 0.9357151229638154266, 1.000000000000000000 ),
 ( 0.000000000000000000, 1.000000000000000000 ),
 .UNSPECIFIED. ) ;
#10201 = FACE_OUTER_BOUND ( 'NONE', #536, .T. ) ;
#10202 = CARTESIAN_POINT ( 'NONE',  ( 9.445361748092775400, 99.50000000000001421, 19.75398588445988324 ) ) ;
#10203 = FACE_BOUND ( 'NONE', #745, .T. ) ;
#10204 = EDGE_LOOP ( 'NONE', ( #6795, #585, #10230, #5353 ) ) ;
#10205 = CARTESIAN_POINT ( 'NONE',  ( -15.84348323231452049, 99.50000000000000000, 15.18005498687102772 ) ) ;
#10206 = CARTESIAN_POINT ( 'NONE',  ( 19.39806930854668110, 1.249999998907525223, -19.39806930854668110 ) ) ;
#10207 = ORIENTED_EDGE ( 'NONE', *, *, #8993, .F. ) ;
#10208 = CARTESIAN_POINT ( 'NONE',  ( -2.499999999999999556, -3.112499999999999822, 1.443375672974065882 ) ) ;
#10209 = DIRECTION ( 'NONE',  ( 0.000000000000000000, 0.000000000000000000, -1.000000000000000000 ) ) ;
#10210 =( BOUNDED_CURVE ( )  B_SPLINE_CURVE ( 2, ( #6762, #8502, #3742, #2963, #6924, #6817, #10124, #6142, #601, #2795, #9340, #2170, #5982, #3798, #5193, #8392, #4414, #6408, #3174, #4782, #9648, #2380, #2330, #4053, #7035, #5577, #1537, #7189, #7236, #9552, #9452, #5677, #1491, #9598, #4687, #8720, #6254, #6460, #2429, #2484, #7137, #8765, #4733, #7086, #7873, #706, #3899, #5625, #8865, #1590, #1691, #9505, #7927, #18, #3953, #10291, #3124, #6309, #1644, #4887, #8815, #7978, #759, #8082, #10342, #5527, #3848, #811, #6358, #5477, #10237, #2281, #4836, #8669, #8030, #863, #4005, #3219, #3070, #75, #3267, #4152, #7381, #2534, #6648, #2673, #3404, #9061, #9840, #5772, #8274, #3315, #4296, #3508, #128, #1054, #6694, #6504, #9694, #219, #5819 ),
 .UNSPECIFIED., .F., .T. ) 
 B_SPLINE_CURVE_WITH_KNOTS ( ( 3, 2, 2, 2, 2, 2, 2, 2, 2, 2, 2, 2, 2, 2, 2, 2, 2, 2, 2, 2, 2, 2, 2, 2, 2, 2, 2, 2, 2, 2, 2, 2, 2, 2, 2, 2, 2, 2, 2, 2, 2, 2, 2, 2, 2, 2, 2, 2, 2, 2, 3 ),
 ( 0.000000000000000000, 0.01785714285714285615, 0.03571428571428571230, 0.05357142857142856845, 0.07142857142857142461, 0.08928571428571428770, 0.1071428571428571369, 0.1250000000000000000, 0.1428571428571428492, 0.1607142857142857262, 0.1785714285714285754, 0.1964285714285714246, 0.2142857142857142738, 0.2321428571428571508, 0.2500000000000000000, 0.2678571428571428492, 0.2857142857142856984, 0.3035714285714285476, 0.3214285714285714524, 0.3392857142857143016, 0.3571428571428571508, 0.3750000000000000000, 0.3928571428571428492, 0.4107142857142856984, 0.4285714285714285476, 0.4464285714285714524, 0.4642857142857143016, 0.4821428571428571508, 0.5000000000000000000, 0.5178571428571429047, 0.5357142857142856984, 0.5535714285714286031, 0.5714285714285713969, 0.5892857142857143016, 0.6071428571428570953, 0.6250000000000000000, 0.6428571428571429047, 0.6607142857142856984, 0.6785714285714286031, 0.6964285714285715079, 0.7142857142857143016, 0.7321428571428570953, 0.7500000000000000000, 0.7678571428571429047, 0.7857142857142856984, 0.8035714285714286031, 0.8214285714285713969, 0.8392857142857143016, 0.8571428571428570953, 0.8750000000000000000, 0.8928571428571429047 ),
 .UNSPECIFIED. ) 
 CURVE ( )  GEOMETRIC_REPRESENTATION_ITEM ( )  RATIONAL_B_SPLINE_CURVE ( ( 1.000000000000000000, 0.9238795325112867385, 1.000000000000000000, 0.9238795325112867385, 1.000000000000000000, 0.9238795325112867385, 1.000000000000000000, 0.9238795325112867385, 1.000000000000000000, 0.9238795325112867385, 1.000000000000000000, 0.9238795325112867385, 1.000000000000000000, 0.9238795325112867385, 1.000000000000000000, 0.9238795325112867385, 1.000000000000000000, 0.9238795325112867385, 1.000000000000000000, 0.9238795325112867385, 1.000000000000000000, 0.9238795325112867385, 1.000000000000000000, 0.9238795325112867385, 1.000000000000000000, 0.9238795325112867385, 1.000000000000000000, 0.9238795325112867385, 1.000000000000000000, 0.9238795325112867385, 1.000000000000000000, 0.9238795325112867385, 1.000000000000000000, 0.9238795325112867385, 1.000000000000000000, 0.9238795325112867385, 1.000000000000000000, 0.9238795325112867385, 1.000000000000000000, 0.9238795325112867385, 1.000000000000000000, 0.9238795325112867385, 1.000000000000000000, 0.9238795325112867385, 1.000000000000000000, 0.9238795325112867385, 1.000000000000000000, 0.9238795325112867385, 1.000000000000000000, 0.9238795325112867385, 1.000000000000000000, 0.9238795325112867385, 1.000000000000000000, 0.9238795325112867385, 1.000000000000000000, 0.9238795325112867385, 1.000000000000000000, 0.9238795325112867385, 1.000000000000000000, 0.9238795325112867385, 1.000000000000000000, 0.9238795325112867385, 1.000000000000000000, 0.9238795325112867385, 1.000000000000000000, 0.9238795325112867385, 1.000000000000000000, 0.9238795325112867385, 1.000000000000000000, 0.9238795325112867385, 1.000000000000000000, 0.9238795325112867385, 1.000000000000000000, 0.9238795325112867385, 1.000000000000000000, 0.9238795325112867385, 1.000000000000000000, 0.9238795325112867385, 1.000000000000000000, 0.9238795325112867385, 1.000000000000000000, 0.9238795325112867385, 1.000000000000000000, 0.9238795325112867385, 1.000000000000000000, 0.9238795325112867385, 1.000000000000000000, 0.9238795325112867385, 1.000000000000000000, 0.9238795325112867385, 1.000000000000000000, 0.9238795325112867385, 1.000000000000000000, 0.9238795325112867385, 1.000000000000000000, 0.9238795325112867385, 1.000000000000000000, 0.9238795325112867385, 1.000000000000000000, 0.9238795325112867385, 1.000000000000000000 ) ) 
 REPRESENTATION_ITEM ( '' )  );
#10211 = CARTESIAN_POINT ( 'NONE',  ( 4.786228327491941173E-16, -1.490624999385482985, 2.605501347177161087 ) ) ;
#10212 = CARTESIAN_POINT ( 'NONE',  ( -11.36312591709337383, 4.799999998907525267, 27.43301269999999548 ) ) ;
#10213 = CARTESIAN_POINT ( 'NONE',  ( -27.43301270000000258, 2.299999998907525267, -11.36312591709336317 ) ) ;
#10214 = ORIENTED_EDGE ( 'NONE', *, *, #8907, .T. ) ;
#10215 = UNCERTAINTY_MEASURE_WITH_UNIT (LENGTH_MEASURE( 1.000000000000000082E-05 ), #2949, 'distance_accuracy_value', 'NONE');
#10216 = CARTESIAN_POINT ( 'NONE',  ( -16.56926954694585774, 100.0000000000000142, 15.12296757606276643 ) ) ;
#10217 = CARTESIAN_POINT ( 'NONE',  ( -2.449293598294706513E-15, 85.00000000000000000, 20.00000000000000000 ) ) ;
#10218 = LINE ( 'NONE', #4555, #2229 ) ;
#10219 = CARTESIAN_POINT ( 'NONE',  ( -15.34161522349497808, 99.99999999999998579, 15.37783959465231121 ) ) ;
#10220 = PRESENTATION_LAYER_ASSIGNMENT (  '', '', ( #4352 ) ) ;
#10221 = CARTESIAN_POINT ( 'NONE',  ( -2.256430356250000102, -0.1781249993854829572, -1.302750673588580321 ) ) ;
#10222 = CARTESIAN_POINT ( 'NONE',  ( 4.504418077186241653, 100.0000000000000426, -21.31258943653750393 ) ) ;
#10223 = ORIENTED_EDGE ( 'NONE', *, *, #1907, .F. ) ;
#10224 = CARTESIAN_POINT ( 'NONE',  ( 2.256430356250000546, -1.303124999385482985, 1.302750673588579877 ) ) ;
#10225 = CARTESIAN_POINT ( 'NONE',  ( -19.39806930854668465, 3.949999998907525178, 19.39806930854667755 ) ) ;
#10226 = DIRECTION ( 'NONE',  ( 0.9853569121566161382, 0.000000000000000000, 0.1705044153832351028 ) ) ;
#10227 = EDGE_CURVE ( 'NONE', #5876, #2327, #5321, .T. ) ;
#10228 = CARTESIAN_POINT ( 'NONE',  ( -11.18376618407356560, 2.649999999999999911, -27.00000000000000355 ) ) ;
#10229 = CARTESIAN_POINT ( 'NONE',  ( 8.901217755223779449, 99.50000000000004263, 19.92336871027421097 ) ) ;
#10230 = ORIENTED_EDGE ( 'NONE', *, *, #10190, .T. ) ;
#10231 = CARTESIAN_POINT ( 'NONE',  ( -27.00000000000001421, 2.850000000000000089, 11.18376618407356560 ) ) ;
#10232 = CARTESIAN_POINT ( 'NONE',  ( -20.96643530928959365, 99.50000000000000000, -10.05541671241504886 ) ) ;
#10233 = ORIENTED_EDGE ( 'NONE', *, *, #6559, .F. ) ;
#10234 = CARTESIAN_POINT ( 'NONE',  ( -1.595409442497313560E-16, -3.515624999385482674, -2.605501347177161087 ) ) ;
#10235 = VERTEX_POINT ( 'NONE', #4270 ) ;
#10236 = ORIENTED_EDGE ( 'NONE', *, *, #1731, .T. ) ;
#10237 = CARTESIAN_POINT ( 'NONE',  ( -19.39806930854667755, 3.749999998907525445, -19.39806930854668110 ) ) ;
#10238 = VECTOR ( 'NONE', #6518, 1000.000000000000000 ) ;
#10239 = CARTESIAN_POINT ( 'NONE',  ( 0.000000000000000000, 0.000000000000000000, -2.500000000000000000 ) ) ;
#10240 = CARTESIAN_POINT ( 'NONE',  ( 2.256430356249999658, -0.4406249993854829961, -1.302750673588581432 ) ) ;
#10241 = CARTESIAN_POINT ( 'NONE',  ( 4.988497440555089923, 99.50000000000000000, -24.29977663856455194 ) ) ;
#10242 = ADVANCED_FACE ( 'NONE', ( #2002 ), #3645, .T. ) ;
#10243 = DIRECTION ( 'NONE',  ( 0.000000000000000000, 0.000000000000000000, -1.000000000000000000 ) ) ;
#10244 = AXIS2_PLACEMENT_3D ( 'NONE', #7931, #4787, #9509 ) ;
#10245 = EDGE_CURVE ( 'NONE', #7989, #4244, #8818, .T. ) ;
#10246 = CARTESIAN_POINT ( 'NONE',  ( 2.500000000000000444, -2.456249998770965615, 1.443375672974063439 ) ) ;
#10247 = PRODUCT_RELATED_PRODUCT_CATEGORY ( 'part', '', ( #1592 ) ) ;
#10248 = CARTESIAN_POINT ( 'NONE',  ( 4.034460619503033030, 99.99999999999995737, -21.08676866017170681 ) ) ;
#10249 = CARTESIAN_POINT ( 'NONE',  ( -22.08823018108446234, 99.50000000000000000, -9.406177930363766038 ) ) ;
#10250 = EDGE_LOOP ( 'NONE', ( #4860, #9917, #4382, #8593 ) ) ;
#10251 = EDGE_CURVE ( 'NONE', #358, #8208, #4387, .T. ) ;
#10252 = CARTESIAN_POINT ( 'NONE',  ( 8.751508028230254865, 99.49999999999998579, 19.58480916780017722 ) ) ;
#10253 = CARTESIAN_POINT ( 'NONE',  ( -2.256430356249999214, -1.003124999385482718, 1.302750673588581876 ) ) ;
#10254 = AXIS2_PLACEMENT_3D ( 'NONE', #317, #1980, #7477 ) ;
#10255 = EDGE_CURVE ( 'NONE', #5851, #2954, #6936, .T. ) ;
#10256 = ORIENTED_EDGE ( 'NONE', *, *, #1716, .T. ) ;
#10257 = DIRECTION ( 'NONE',  ( -1.000000000000000000, 0.000000000000000000, 0.000000000000000000 ) ) ;
#10258 = CARTESIAN_POINT ( 'NONE',  ( 9.600410285814406919, 99.49999999999998579, 19.87914582625927196 ) ) ;
#10259 = CARTESIAN_POINT ( 'NONE',  ( 24.93339342948717885, 100.0000000000000000, -1.235376602564102644 ) ) ;
#10260 = ORIENTED_EDGE ( 'NONE', *, *, #6453, .F. ) ;
#10261 = CARTESIAN_POINT ( 'NONE',  ( -15.69732130854469432, 100.0000000000000142, 15.19348709373450035 ) ) ;
#10262 = AXIS2_PLACEMENT_3D ( 'NONE', #7450, #2432, #4890 ) ;
#10263 = CARTESIAN_POINT ( 'NONE',  ( -19.39806930854668465, 4.049999998907525267, 19.39806930854667755 ) ) ;
#10264 = ORIENTED_EDGE ( 'NONE', *, *, #2448, .F. ) ;
#10265 = CARTESIAN_POINT ( 'NONE',  ( 2.500000000000000444, -4.762499999999999289, 1.443375672974063439 ) ) ;
#10266 = CARTESIAN_POINT ( 'NONE',  ( 3.764204346677844093, 100.0000000000000142, -22.52576385118515745 ) ) ;
#10267 = CARTESIAN_POINT ( 'NONE',  ( 2.256430356250000102, -0.3656249993854829294, -2.763330213280484622E-16 ) ) ;
#10268 = CARTESIAN_POINT ( 'NONE',  ( 4.829054701479813083, 99.50000000000000000, -23.91032069601275367 ) ) ;
#10269 = CARTESIAN_POINT ( 'NONE',  ( 1.679787559701184688E-15, 3.749999998907525445, -27.43301270000000258 ) ) ;
#10270 = COLOUR_RGB ( '',0.8941176470588234615, 0.8941176470588234615, 0.8941176470588234615 ) ;
#10271 = CARTESIAN_POINT ( 'NONE',  ( -15.30604604128650692, 99.99999999999997158, 15.41317891555018349 ) ) ;
#10272 = DIRECTION ( 'NONE',  ( 0.08704561088320923734, 0.9949358851208914833, 0.05025580687519627665 ) ) ;
#10273 = CARTESIAN_POINT ( 'NONE',  ( -16.56928979259283352, 99.50000000000002842, 16.65656195153832897 ) ) ;
#10274 = CARTESIAN_POINT ( 'NONE',  ( 11.18376618407357626, 3.850000000000000089, 27.00000000000000000 ) ) ;
#10275 = CARTESIAN_POINT ( 'NONE',  ( 2.256430356249999658, -4.828124999385482674, -1.302750673588581432 ) ) ;
#10276 = CARTESIAN_POINT ( 'NONE',  ( 3.712044765110731337, 99.49999999999998579, -21.08683700305641651 ) ) ;
#10277 = ORIENTED_EDGE ( 'NONE', *, *, #7602, .F. ) ;
#10278 = VERTEX_POINT ( 'NONE', #2180 ) ;
#10279 = CARTESIAN_POINT ( 'NONE',  ( 1.128215178124999607, -2.090624999385482852, -1.954126010382871259 ) ) ;
#10280 =( BOUNDED_CURVE ( )  B_SPLINE_CURVE ( 2, ( #7045, #10198, #7724, #7098, #5322, #3184, #10303, #4528, #6155 ),
 .UNSPECIFIED., .F., .T. ) 
 B_SPLINE_CURVE_WITH_KNOTS ( ( 3, 2, 2, 2, 3 ),
 ( 0.7291666666666667407, 0.7361111111111111605, 0.7500000000000000000, 0.7638888888888888395, 0.7708333333333333703 ),
 .UNSPECIFIED. ) 
 CURVE ( )  GEOMETRIC_REPRESENTATION_ITEM ( )  RATIONAL_B_SPLINE_CURVE ( ( 0.9330127018922192983, 0.9330127018922198534, 1.000000000000000000, 0.8660254037844387076, 1.000000000000000000, 0.8660254037844387076, 1.000000000000000000, 0.9330127018922187432, 0.9330127018922192983 ) ) 
 REPRESENTATION_ITEM ( '' )  );
#10281 = CARTESIAN_POINT ( 'NONE',  ( -27.43301270000000258, 1.549999998907525267, -3.359575119402369376E-15 ) ) ;
#10282 = CARTESIAN_POINT ( 'NONE',  ( 3.681717055787076642, 99.50000000000000000, -21.09125273517263111 ) ) ;
#10283 = FACE_OUTER_BOUND ( 'NONE', #2315, .T. ) ;
#10284 = CARTESIAN_POINT ( 'NONE',  ( 9.245739950628269810, 99.50000000000002842, 20.03726560014620617 ) ) ;
#10285 = ORIENTED_EDGE ( 'NONE', *, *, #3357, .F. ) ;
#10286 = CARTESIAN_POINT ( 'NONE',  ( -16.56313167360273297, 99.99999999999998579, 16.06491815633068398 ) ) ;
#10287 = CARTESIAN_POINT ( 'NONE',  ( 8.337740814200648387, 100.0000000000000284, 20.10843643765939248 ) ) ;
#10288 = CARTESIAN_POINT ( 'NONE',  ( -2.256430356250000102, -3.403124999385482408, 0.000000000000000000 ) ) ;
#10289 = EDGE_LOOP ( 'NONE', ( #6164, #2635, #6864, #8774 ) ) ;
#10290 = EDGE_CURVE ( 'NONE', #10048, #1242, #3270, .T. ) ;
#10291 = CARTESIAN_POINT ( 'NONE',  ( -27.43301270000000258, 2.999999998907525445, -11.36312591709336317 ) ) ;
#10292 = DIRECTION ( 'NONE',  ( 0.000000000000000000, 0.000000000000000000, -1.000000000000000000 ) ) ;
#10293 = B_SPLINE_SURFACE_WITH_KNOTS ( 'NONE', 3, 1, ( 
 ( #7670, #561 ),
 ( #6045, #398 ),
 ( #2125, #7143 ),
 ( #10024, #3701 ),
 ( #1182, #6883 ),
 ( #5325, #9975 ),
 ( #2916, #8515 ),
 ( #1343, #2859 ),
 ( #7559, #4530 ),
 ( #7727, #1544 ),
 ( #5995, #3179 ),
 ( #3754, #9234 ),
 ( #9186, #10140 ),
 ( #2066, #2977 ),
 ( #6158, #9354 ) ),
 .UNSPECIFIED., .F., .F., .F.,
 ( 4, 1, 1, 1, 1, 1, 1, 1, 1, 1, 1, 1, 4 ),
 ( 2, 2 ),
 ( 0.000000000000000000, 0.09895296010982183865, 0.1966578232739713550, 0.2939931048315790330, 0.3929322324600736938, 0.4463669803336778319, 0.5055752425223922764, 0.5715235163887821823, 0.6440401046887170855, 0.7229629404452876384, 0.8087840669208056221, 0.9009145765370688563, 1.000000000000000000 ),
 ( 0.000000000000000000, 1.000000000000000000 ),
 .UNSPECIFIED. ) ;
#10294 = CARTESIAN_POINT ( 'NONE',  ( 2.256430356250000102, -0.4781249993854829183, -2.763330213280484622E-16 ) ) ;
#10295 = CARTESIAN_POINT ( 'NONE',  ( -16.52319226728147328, 99.99999999999998579, 15.63609008536095324 ) ) ;
#10296 = DIRECTION ( 'NONE',  ( -0.000000000000000000, 1.000000000000000000, -0.000000000000000000 ) ) ;
#10297 = CARTESIAN_POINT ( 'NONE',  ( -1.767625397874844694E-16, -2.756249998770965437, -2.886751345948128655 ) ) ;
#10298 = EDGE_LOOP ( 'NONE', ( #9451, #5155, #3515, #5700 ) ) ;
#10299 = EDGE_CURVE ( 'NONE', #4436, #5524, #7324, .T. ) ;
#10300 = ADVANCED_FACE ( 'NONE', ( #763 ), #7723, .T. ) ;
#10301 = CARTESIAN_POINT ( 'NONE',  ( 4.835062408351179286, 100.0000000000000000, -21.79588013901878440 ) ) ;
#10302 = CARTESIAN_POINT ( 'NONE',  ( -15.24337324910153946, 99.99999999999997158, 16.81353386054630761 ) ) ;
#10303 = CARTESIAN_POINT ( 'NONE',  ( -1.250000000000000222, -4.518749998770965171, -2.165063509461096825 ) ) ;
#10304 = CARTESIAN_POINT ( 'NONE',  ( 4.786228327491941173E-16, -2.278124999385482852, 2.605501347177161087 ) ) ;
#10305 = CARTESIAN_POINT ( 'NONE',  ( 23.82500000000000284, 72.50000000000001421, -2.917720998968569322E-15 ) ) ;
#10306 = LINE ( 'NONE', #2299, #7198 ) ;
#10307 = ORIENTED_EDGE ( 'NONE', *, *, #839, .F. ) ;
#10308 = CARTESIAN_POINT ( 'NONE',  ( -17.94007301623892658, 99.50000000000000000, 17.49000340848992607 ) ) ;
#10309 = CARTESIAN_POINT ( 'NONE',  ( -19.39806930854667755, 4.649999998907525800, -19.39806930854668110 ) ) ;
#10310 = EDGE_LOOP ( 'NONE', ( #7436, #2855, #5362, #10109, #9437, #1643, #9608, #73, #7696, #3118, #2550, #4333, #2912, #1589, #623, #4754, #3516 ) ) ;
#10311 = CARTESIAN_POINT ( 'NONE',  ( 1.250000000000001110, -2.999999999999999556, 2.165063509461096380 ) ) ;
#10312 = CONTEXT_DEPENDENT_SHAPE_REPRESENTATION ( #5994, #2067 ) ;
#10313 = VECTOR ( 'NONE', #3183, 1000.000000000000000 ) ;
#10314 = CARTESIAN_POINT ( 'NONE',  ( -20.93575003794465061, 100.0000000000000142, -10.12220034237898503 ) ) ;
#10315 = CARTESIAN_POINT ( 'NONE',  ( -2.256430356250000102, -3.890624999385482674, -1.302750673588580321 ) ) ;
#10316 = CARTESIAN_POINT ( 'NONE',  ( -21.12798922145720582, 99.50000000000001421, -10.90888695829967325 ) ) ;
#10317 = CARTESIAN_POINT ( 'NONE',  ( 11.36312591709336850, 4.999999998907526333, 27.43301269999999903 ) ) ;
#10318 = CARTESIAN_POINT ( 'NONE',  ( 6.246869686064662197, 99.50000000000000000, 20.92172973853146090 ) ) ;
#10319 = B_SPLINE_CURVE_WITH_KNOTS ( 'NONE', 3,
 ( #530, #2939, #9317, #6906, #10273, #2204, #7752 ),
 .UNSPECIFIED., .F., .F.,
 ( 4, 1, 1, 1, 4 ),
 ( 0.000000000000000000, 0.2687002788711734813, 0.5225003893189538173, 0.7676814173175746658, 1.000000000000000000 ),
 .UNSPECIFIED. ) ;
#10320 = CARTESIAN_POINT ( 'NONE',  ( 3.664124300404482337, 100.0000000000000284, -24.27219056640880623 ) ) ;
#10321 = FACE_BOUND ( 'NONE', #3680, .T. ) ;
#10322 = ADVANCED_FACE ( 'NONE', ( #1646 ), #9649, .T. ) ;
#10323 = CARTESIAN_POINT ( 'NONE',  ( 3.061616997868383141E-16, 0.000000000000000000, 2.500000000000000000 ) ) ;
#10324 = AXIS2_PLACEMENT_3D ( 'NONE', #9809, #3423, #4172 ) ;
#10325 = CARTESIAN_POINT ( 'NONE',  ( -2.256430356250000102, -2.878124999385482941, -1.302750673588580321 ) ) ;
#10326 = CARTESIAN_POINT ( 'NONE',  ( -21.39817337045129619, 99.50000000000001421, -9.317726141196148504 ) ) ;
#10327 = EDGE_LOOP ( 'NONE', ( #6859, #970, #2513, #8854 ) ) ;
#10328 = EDGE_LOOP ( 'NONE', ( #424, #6968, #3684, #9188 ) ) ;
#10329 = CARTESIAN_POINT ( 'NONE',  ( -2.256430356250000102, -1.078124999385482896, -1.302750673588580321 ) ) ;
#10330 = CARTESIAN_POINT ( 'NONE',  ( -27.43301270000000258, 4.599999998907525978, -11.36312591709336317 ) ) ;
#10331 =( LENGTH_UNIT ( ) NAMED_UNIT ( * ) SI_UNIT ( .MILLI., .METRE. ) );
#10332 = CARTESIAN_POINT ( 'NONE',  ( 0.000000000000000000, 0.000000000000000000, 0.000000000000000000 ) ) ;
#10333 = CARTESIAN_POINT ( 'NONE',  ( 19.39806930854668110, 1.149999998907525356, -19.39806930854668110 ) ) ;
#10334 = CARTESIAN_POINT ( 'NONE',  ( 9.877377282685029372E-16, -3.431249998770965259, 2.500000000000000000 ) ) ;
#10335 =( GEOMETRIC_REPRESENTATION_CONTEXT ( 3 ) GLOBAL_UNCERTAINTY_ASSIGNED_CONTEXT ( ( #7690 ) ) GLOBAL_UNIT_ASSIGNED_CONTEXT ( ( #1042, #9730, #8950 ) ) REPRESENTATION_CONTEXT ( 'NONE', 'WORKASPACE' ) );
#10336 = ORIENTED_EDGE ( 'NONE', *, *, #4623, .T. ) ;
#10337 = DIRECTION ( 'NONE',  ( -0.000000000000000000, 1.000000000000000000, -0.000000000000000000 ) ) ;
#10338 = CARTESIAN_POINT ( 'NONE',  ( 8.149445629999579666, 100.0000000000000284, 20.33980848884064230 ) ) ;
#10339 =( BOUNDED_CURVE ( )  B_SPLINE_CURVE ( 2, ( #6290, #10274, #6342, #2413, #9537, #7859, #5558, #1626, #1574 ),
 .UNSPECIFIED., .F., .T. ) 
 B_SPLINE_CURVE_WITH_KNOTS ( ( 3, 2, 2, 2, 3 ),
 ( 0.6785714285714286031, 0.6964285714285713969, 0.7142857142857143016, 0.7321428571428570953, 0.7500000000000000000 ),
 .UNSPECIFIED. ) 
 CURVE ( )  GEOMETRIC_REPRESENTATION_ITEM ( )  RATIONAL_B_SPLINE_CURVE ( ( 1.000000000000000000, 0.9238795325112867385, 1.000000000000000000, 0.9238795325112867385, 1.000000000000000000, 0.9238795325112867385, 1.000000000000000000, 0.9238795325112867385, 1.000000000000000000 ) ) 
 REPRESENTATION_ITEM ( '' )  );
#10340 = CARTESIAN_POINT ( 'NONE',  ( 2.256430356250000546, -4.115624999385482319, 1.302750673588579877 ) ) ;
#10341 = CARTESIAN_POINT ( 'NONE',  ( 0.6698729810778025762, -5.211153809338632037, 2.500000000000002665 ) ) ;
#10342 = CARTESIAN_POINT ( 'NONE',  ( 27.43301270000000258, 3.449999998907525178, 0.000000000000000000 ) ) ;
#10343 = CARTESIAN_POINT ( 'NONE',  ( 4.135809822336132591, 99.99999999999998579, -24.70305975188825443 ) ) ;
#10344 = CARTESIAN_POINT ( 'NONE',  ( -3.486133158594716510E-16, -1.012499999999999956, -2.500000000000000000 ) ) ;
#10345 = AXIS2_PLACEMENT_3D ( 'NONE', #9982, #3817, #7566 ) ;
#10346 = CARTESIAN_POINT ( 'NONE',  ( -1.128215178125000273, -4.378124999385482496, -1.954126010382871259 ) ) ;
#10347 = CARTESIAN_POINT ( 'NONE',  ( 3.079986699855593473E-15, 100.0000000000000000, 25.15000000000000213 ) ) ;
#10348 = CARTESIAN_POINT ( 'NONE',  ( -16.70213339477928471, 99.49999999999998579, 16.52464093453885852 ) ) ;
#10349 = CARTESIAN_POINT ( 'NONE',  ( 2.143131898507868643E-15, 105.0000000000000142, 17.50000000000000355 ) ) ;
#10350 = AXIS2_PLACEMENT_3D ( 'NONE', #3654, #6834, #3705 ) ;
#10351 = CARTESIAN_POINT ( 'NONE',  ( 1.250000000000001110, -1.143749998770965837, 2.165063509461096380 ) ) ;
#10352 = CARTESIAN_POINT ( 'NONE',  ( 0.000000000000000000, 71.18660744634364335, 23.99999999999999645 ) ) ;
#10353 = LINE ( 'NONE', #2394, #10313 ) ;
#10354 = CARTESIAN_POINT ( 'NONE',  ( -7.500000000000000000, 105.0000000000000142, -3.000000000000000000 ) ) ;
#10355 = CARTESIAN_POINT ( 'NONE',  ( -2.256430356249999214, -5.053124999385482319, 1.302750673588581876 ) ) ;
#10356 = ADVANCED_FACE ( 'NONE', ( #7929 ), #762, .T. ) ;
#10357 = ORIENTED_EDGE ( 'NONE', *, *, #531, .F. ) ;
#10358 = CARTESIAN_POINT ( 'NONE',  ( 2.928963527206765338, 99.49999999999997158, -23.52685633767685758 ) ) ;
#10359 = ORIENTED_EDGE ( 'NONE', *, *, #4869, .T. ) ;
#10360 = CYLINDRICAL_SURFACE ( 'NONE', #1116, 18.00000000000000000 ) ;
#10361 = CARTESIAN_POINT ( 'NONE',  ( 0.6698729810778087934, -1.876346188203300347, -2.499999999999999112 ) ) ;
#10362 = B_SPLINE_CURVE_WITH_KNOTS ( 'NONE', 3,
 ( #9711, #7396, #7253, #94, #5696, #1950, #7550, #700, #9446, #9129, #2218, #4680, #3583, #7820, #8610, #2955, #7496, #6304, #9389 ),
 .UNSPECIFIED., .F., .F.,
 ( 4, 1, 1, 1, 1, 1, 1, 1, 1, 1, 1, 1, 1, 1, 1, 1, 4 ),
 ( 0.000000000000000000, 0.06473908249738200005, 0.1274869542813800993, 0.1888754624962200035, 0.2498352098569301405, 0.3101749858420705941, 0.3718734486855839183, 0.4342313324889700565, 0.4990836447755341299, 0.5639614065304963120, 0.6264045329497629488, 0.6882484937299673255, 0.7493615009078817835, 0.8100377551054726011, 0.8717391907241844873, 0.9348513958286107650, 1.000000000000000000 ),
 .UNSPECIFIED. ) ;
#10363 = CARTESIAN_POINT ( 'NONE',  ( 7.826802610544922878, 99.50000000000000000, 21.21129867192371421 ) ) ;
#10364 = CARTESIAN_POINT ( 'NONE',  ( -19.39806930854668465, 3.249999998907525001, 19.39806930854667755 ) ) ;
#10365 = ORIENTED_EDGE ( 'NONE', *, *, #4409, .F. ) ;
#10366 = CARTESIAN_POINT ( 'NONE',  ( -15.76250887235353737, 99.49999999999998579, 16.65066592061022277 ) ) ;
#10367 = NEXT_ASSEMBLY_USAGE_OCCURRENCE ( 'NAUO1', ' ', ' ', #2372, #2680, $ ) ;
#10368 = NEXT_ASSEMBLY_USAGE_OCCURRENCE ( 'NAUO2', ' ', ' ', #2372, #3442, $ ) ;
#10369 = NEXT_ASSEMBLY_USAGE_OCCURRENCE ( 'NAUO3', ' ', ' ', #2372, #4215, $ ) ;
#10370 = NEXT_ASSEMBLY_USAGE_OCCURRENCE ( 'NAUO4', ' ', ' ', #2372, #3149, $ ) ;
#10371 = NEXT_ASSEMBLY_USAGE_OCCURRENCE ( 'NAUO5', ' ', ' ', #2372, #1142, $ ) ;
#10372 = NEXT_ASSEMBLY_USAGE_OCCURRENCE ( 'NAUO6', ' ', ' ', #2372, #8713, $ ) ;
#10373 = NEXT_ASSEMBLY_USAGE_OCCURRENCE ( 'NAUO7', ' ', ' ', #2372, #7805, $ ) ;
#10374=COLOUR_RGB('Dark Blue',0.08,0.2,0.34);
#10375=FILL_AREA_STYLE_COLOUR('',#10374);
#10376=FILL_AREA_STYLE('',(#10375));
#10377=SURFACE_STYLE_FILL_AREA(#10376);
#10378=SURFACE_SIDE_STYLE('',(#10377));
#10379=SURFACE_STYLE_USAGE(.BOTH.,#10378);
#10380=PRESENTATION_STYLE_ASSIGNMENT((#10379));
#10381=COLOUR_RGB('Light Blue',0.38,0.62,0.78);
#10382=FILL_AREA_STYLE_COLOUR('',#10381);
#10383=FILL_AREA_STYLE('',(#10382));
#10384=SURFACE_STYLE_FILL_AREA(#10383);
#10385=SURFACE_SIDE_STYLE('',(#10384));
#10386=SURFACE_STYLE_USAGE(.BOTH.,#10385);
#10387=PRESENTATION_STYLE_ASSIGNMENT((#10386));
#10388=COLOUR_RGB('Sky Blue',0.24,0.69,0.87);
#10389=FILL_AREA_STYLE_COLOUR('',#10388);
#10390=FILL_AREA_STYLE('',(#10389));
#10391=SURFACE_STYLE_FILL_AREA(#10390);
#10392=SURFACE_SIDE_STYLE('',(#10391));
#10393=SURFACE_STYLE_USAGE(.BOTH.,#10392);
#10394=PRESENTATION_STYLE_ASSIGNMENT((#10393));
#10395=COLOUR_RGB('Grey',0.48,0.52,0.57);
#10396=FILL_AREA_STYLE_COLOUR('',#10395);
#10397=FILL_AREA_STYLE('',(#10396));
#10398=SURFACE_STYLE_FILL_AREA(#10397);
#10399=SURFACE_SIDE_STYLE('',(#10398));
#10400=SURFACE_STYLE_USAGE(.BOTH.,#10399);
#10401=PRESENTATION_STYLE_ASSIGNMENT((#10400));
#10402=COLOUR_RGB('Black',0.12,0.14,0.17);
#10403=FILL_AREA_STYLE_COLOUR('',#10402);
#10404=FILL_AREA_STYLE('',(#10403));
#10405=SURFACE_STYLE_FILL_AREA(#10404);
#10406=SURFACE_SIDE_STYLE('',(#10405));
#10407=SURFACE_STYLE_USAGE(.BOTH.,#10406);
#10408=PRESENTATION_STYLE_ASSIGNMENT((#10407));
#10409=COLOUR_RGB('Off White',0.89,0.88,0.83);
#10410=FILL_AREA_STYLE_COLOUR('',#10409);
#10411=FILL_AREA_STYLE('',(#10410));
#10412=SURFACE_STYLE_FILL_AREA(#10411);
#10413=SURFACE_SIDE_STYLE('',(#10412));
#10414=SURFACE_STYLE_USAGE(.BOTH.,#10413);
#10415=PRESENTATION_STYLE_ASSIGNMENT((#10414));
ENDSEC;
END-ISO-10303-21;
